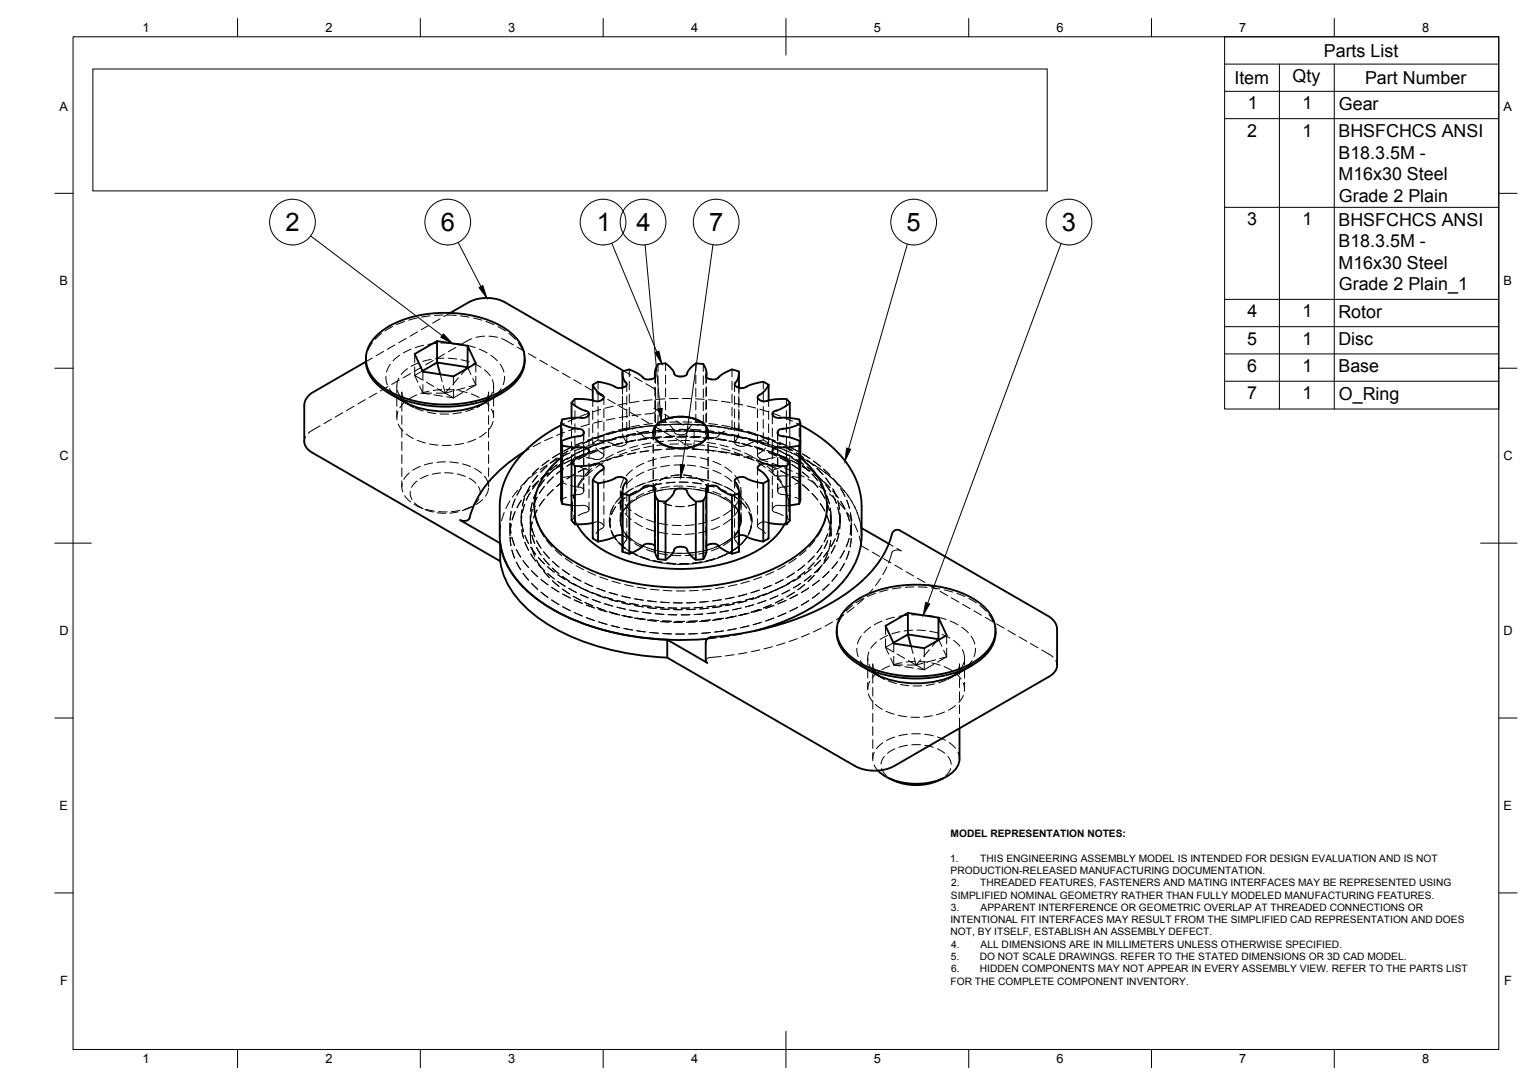
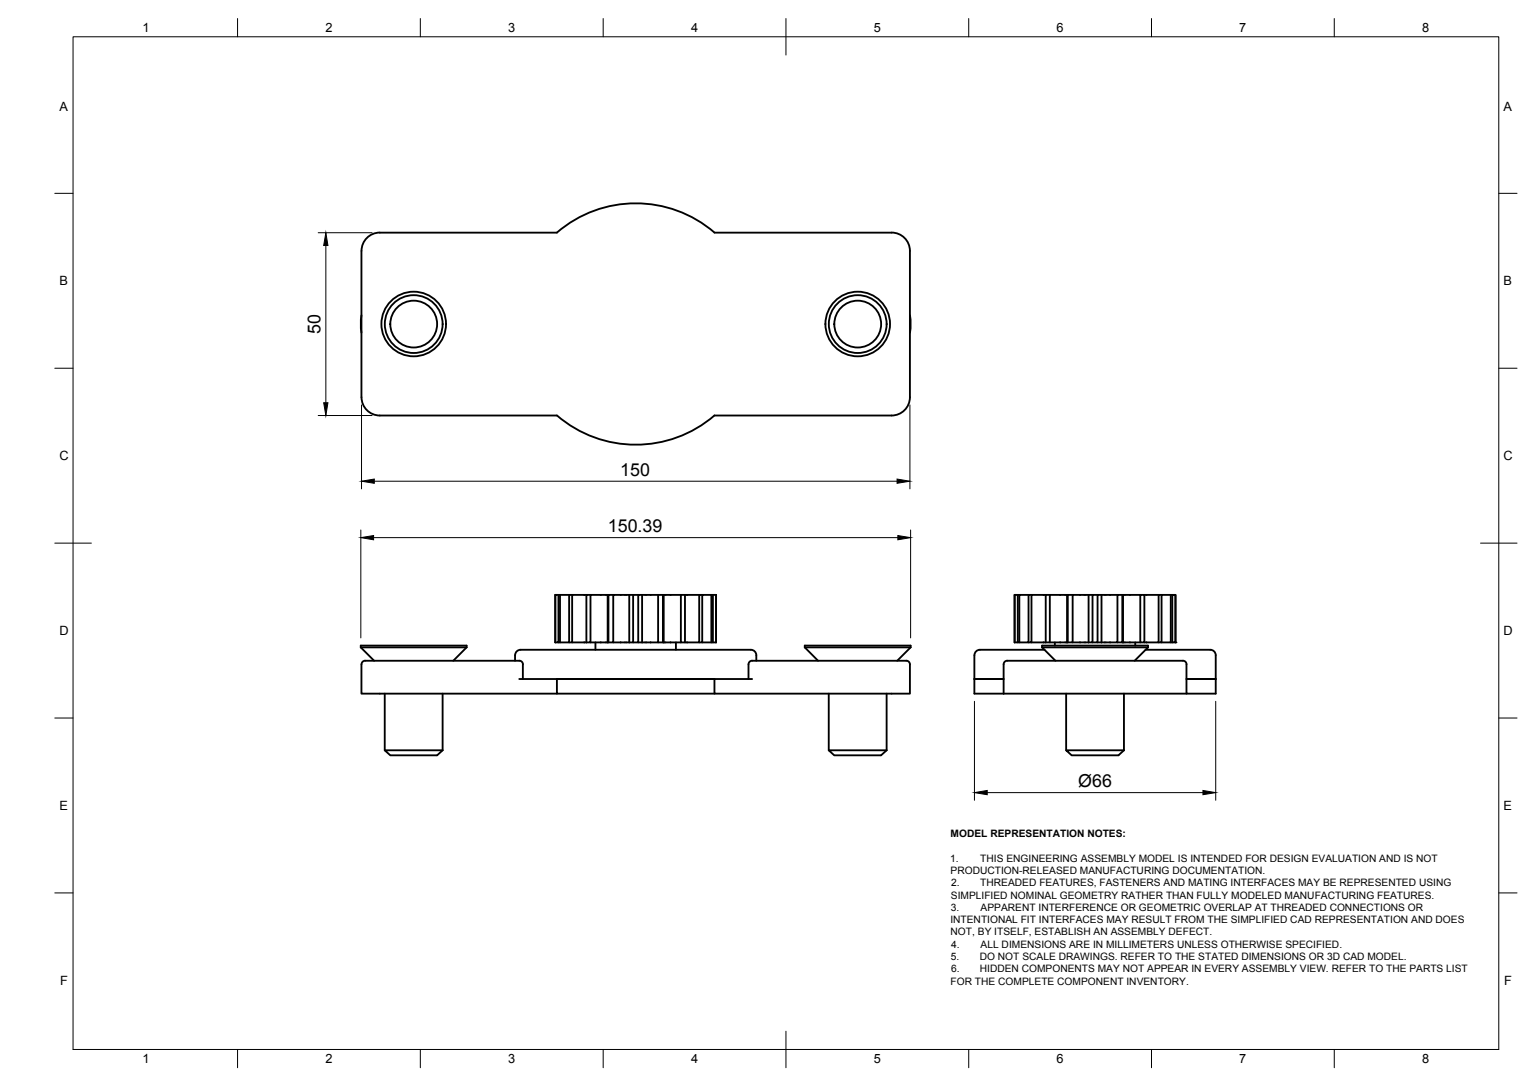
ISO-10303-21;
HEADER;
/* Generated by software containing ST-Developer
 * from STEP Tools, Inc. (www.steptools.com) 
 */

FILE_DESCRIPTION(
/* description */ (''),
/* implementation_level */ '2;1');

FILE_NAME(
/* name */ 'BR-110',
/* time_stamp */ '2026-10-04T22:47:03-07:00',
/* author */ (''),
/* organization */ (''),
/* preprocessor_version */ 'ST-DEVELOPER v20.2',
/* originating_system */ 'Autodesk Translation Framework v15.15.0.0',
/* authorisation */ '');

FILE_SCHEMA (('AUTOMOTIVE_DESIGN { 1 0 10303 214 3 1 1 }'));
ENDSEC;

DATA;
#10=MECHANICAL_DESIGN_GEOMETRIC_PRESENTATION_REPRESENTATION('',(#77,#78,
#79,#80,#81,#82,#83),#19878);
#11=ITEM_DEFINED_TRANSFORMATION($,$,#4911,#5420);
#12=ITEM_DEFINED_TRANSFORMATION($,$,#5197,#5421);
#13=ITEM_DEFINED_TRANSFORMATION($,$,#5224,#5422);
#14=ITEM_DEFINED_TRANSFORMATION($,$,#5251,#5423);
#15=ITEM_DEFINED_TRANSFORMATION($,$,#5268,#5424);
#16=ITEM_DEFINED_TRANSFORMATION($,$,#5309,#5425);
#17=ITEM_DEFINED_TRANSFORMATION($,$,#5416,#5426);
#18=(
REPRESENTATION_RELATIONSHIP($,$,#19907,#19906)
REPRESENTATION_RELATIONSHIP_WITH_TRANSFORMATION(#11)
SHAPE_REPRESENTATION_RELATIONSHIP()
);
#19=(
REPRESENTATION_RELATIONSHIP($,$,#19908,#19906)
REPRESENTATION_RELATIONSHIP_WITH_TRANSFORMATION(#12)
SHAPE_REPRESENTATION_RELATIONSHIP()
);
#20=(
REPRESENTATION_RELATIONSHIP($,$,#19909,#19906)
REPRESENTATION_RELATIONSHIP_WITH_TRANSFORMATION(#13)
SHAPE_REPRESENTATION_RELATIONSHIP()
);
#21=(
REPRESENTATION_RELATIONSHIP($,$,#19910,#19906)
REPRESENTATION_RELATIONSHIP_WITH_TRANSFORMATION(#14)
SHAPE_REPRESENTATION_RELATIONSHIP()
);
#22=(
REPRESENTATION_RELATIONSHIP($,$,#19911,#19906)
REPRESENTATION_RELATIONSHIP_WITH_TRANSFORMATION(#15)
SHAPE_REPRESENTATION_RELATIONSHIP()
);
#23=(
REPRESENTATION_RELATIONSHIP($,$,#19912,#19906)
REPRESENTATION_RELATIONSHIP_WITH_TRANSFORMATION(#16)
SHAPE_REPRESENTATION_RELATIONSHIP()
);
#24=(
REPRESENTATION_RELATIONSHIP($,$,#19913,#19906)
REPRESENTATION_RELATIONSHIP_WITH_TRANSFORMATION(#17)
SHAPE_REPRESENTATION_RELATIONSHIP()
);
#25=CONTEXT_DEPENDENT_SHAPE_REPRESENTATION(#18,#19899);
#26=CONTEXT_DEPENDENT_SHAPE_REPRESENTATION(#19,#19900);
#27=CONTEXT_DEPENDENT_SHAPE_REPRESENTATION(#20,#19901);
#28=CONTEXT_DEPENDENT_SHAPE_REPRESENTATION(#21,#19902);
#29=CONTEXT_DEPENDENT_SHAPE_REPRESENTATION(#22,#19903);
#30=CONTEXT_DEPENDENT_SHAPE_REPRESENTATION(#23,#19904);
#31=CONTEXT_DEPENDENT_SHAPE_REPRESENTATION(#24,#19905);
#32=NEXT_ASSEMBLY_USAGE_OCCURRENCE('Gear:1','Gear:1','Gear:1',#19915,#19916,
'Gear:1');
#33=NEXT_ASSEMBLY_USAGE_OCCURRENCE('Screw_02:1','Screw_02:1',
'Screw_02:1',#19915,#19917,'Screw_02:1');
#34=NEXT_ASSEMBLY_USAGE_OCCURRENCE('Screw_01:1','Screw_01:1',
'Screw_01:1',#19915,#19918,'Screw_01:1');
#35=NEXT_ASSEMBLY_USAGE_OCCURRENCE('Rotor:1','Rotor:1','Rotor:1',#19915,
#19919,'Rotor:1');
#36=NEXT_ASSEMBLY_USAGE_OCCURRENCE('Disc:1','Disc:1','Disc:1',#19915,#19920,
'Disc:1');
#37=NEXT_ASSEMBLY_USAGE_OCCURRENCE('Base:1','Base:1','Base:1',#19915,#19921,
'Base:1');
#38=NEXT_ASSEMBLY_USAGE_OCCURRENCE('O_Ring:1','O_Ring:1','O_Ring:1',#19915,
#19922,'O_Ring:1');
#39=SPHERICAL_SURFACE('',#5318,1.);
#40=SPHERICAL_SURFACE('',#5323,1.);
#41=SPHERICAL_SURFACE('',#5367,1.);
#42=SPHERICAL_SURFACE('',#5372,1.);
#43=TOROIDAL_SURFACE('',#5201,8.911,1.);
#44=TOROIDAL_SURFACE('',#5228,8.911,1.);
#45=TOROIDAL_SURFACE('',#5257,12.,1.);
#46=TOROIDAL_SURFACE('',#5269,18.2498324643894,1.5);
#47=TOROIDAL_SURFACE('',#5277,28.1934256722844,1.5);
#48=TOROIDAL_SURFACE('',#5285,31.5,1.5);
#49=TOROIDAL_SURFACE('',#5293,12.,1.);
#50=TOROIDAL_SURFACE('',#5313,39.889325151227,1.);
#51=TOROIDAL_SURFACE('',#5335,4.,1.);
#52=TOROIDAL_SURFACE('',#5340,4.,1.);
#53=TOROIDAL_SURFACE('',#5362,39.889325151227,1.);
#54=TOROIDAL_SURFACE('',#5384,4.,1.);
#55=TOROIDAL_SURFACE('',#5389,4.,1.);
#56=TOROIDAL_SURFACE('',#5417,12.,1.);
#57=CONICAL_SURFACE('',#5198,7.28,0.832981266674429);
#58=CONICAL_SURFACE('',#5205,11.24,0.785398163397495);
#59=CONICAL_SURFACE('',#5225,7.28,0.832981266674429);
#60=CONICAL_SURFACE('',#5232,11.24,0.785398163397495);
#61=CONICAL_SURFACE('',#5342,9.8273485245745,0.785398163397449);
#62=CONICAL_SURFACE('',#5391,9.8273485245745,0.785398163397449);
#63=SHAPE_REPRESENTATION_RELATIONSHIP('SRR','None',#19907,#70);
#64=SHAPE_REPRESENTATION_RELATIONSHIP('SRR','None',#19908,#71);
#65=SHAPE_REPRESENTATION_RELATIONSHIP('SRR','None',#19909,#72);
#66=SHAPE_REPRESENTATION_RELATIONSHIP('SRR','None',#19910,#73);
#67=SHAPE_REPRESENTATION_RELATIONSHIP('SRR','None',#19911,#74);
#68=SHAPE_REPRESENTATION_RELATIONSHIP('SRR','None',#19912,#75);
#69=SHAPE_REPRESENTATION_RELATIONSHIP('SRR','None',#19913,#76);
#70=ADVANCED_BREP_SHAPE_REPRESENTATION('',(#84),#19871);
#71=ADVANCED_BREP_SHAPE_REPRESENTATION('',(#85),#19872);
#72=ADVANCED_BREP_SHAPE_REPRESENTATION('',(#86),#19873);
#73=ADVANCED_BREP_SHAPE_REPRESENTATION('',(#87),#19874);
#74=ADVANCED_BREP_SHAPE_REPRESENTATION('',(#88),#19875);
#75=ADVANCED_BREP_SHAPE_REPRESENTATION('',(#89),#19876);
#76=ADVANCED_BREP_SHAPE_REPRESENTATION('',(#90),#19877);
#77=STYLED_ITEM('',(#19951),#84);
#78=STYLED_ITEM('',(#19952),#85);
#79=STYLED_ITEM('',(#19952),#86);
#80=STYLED_ITEM('',(#19953),#87);
#81=STYLED_ITEM('',(#19954),#88);
#82=STYLED_ITEM('',(#19951),#89);
#83=STYLED_ITEM('',(#19955),#90);
#84=MANIFOLD_SOLID_BREP('Body1',#4825);
#85=MANIFOLD_SOLID_BREP('Body1',#4826);
#86=MANIFOLD_SOLID_BREP('Body1',#4827);
#87=MANIFOLD_SOLID_BREP('Body1',#4828);
#88=MANIFOLD_SOLID_BREP('Body1',#4829);
#89=MANIFOLD_SOLID_BREP('Body1',#4830);
#90=MANIFOLD_SOLID_BREP('Body1',#4831);
#91=FACE_BOUND('',#736,.T.);
#92=FACE_BOUND('',#738,.T.);
#93=FACE_BOUND('',#783,.T.);
#94=FACE_BOUND('',#803,.T.);
#95=FACE_BOUND('',#808,.T.);
#96=FACE_BOUND('',#814,.T.);
#97=FACE_BOUND('',#819,.T.);
#98=FACE_BOUND('',#822,.T.);
#99=FACE_BOUND('',#827,.T.);
#100=FACE_BOUND('',#831,.T.);
#101=FACE_BOUND('',#834,.T.);
#102=FACE_BOUND('',#837,.T.);
#103=FACE_BOUND('',#840,.T.);
#104=FACE_BOUND('',#849,.T.);
#105=FACE_BOUND('',#871,.T.);
#106=FACE_BOUND('',#886,.T.);
#107=FACE_BOUND('',#887,.T.);
#108=FACE_BOUND('',#889,.T.);
#109=FACE_BOUND('',#892,.T.);
#110=FACE_BOUND('',#895,.T.);
#111=B_SPLINE_CURVE_WITH_KNOTS('',5,(#7546,#7547,#7548,#7549,#7550,#7551,
#7552,#7553,#7554,#7555,#7556,#7557,#7558,#7559,#7560,#7561,#7562,#7563,
#7564,#7565,#7566,#7567,#7568,#7569,#7570,#7571,#7572,#7573,#7574,#7575,
#7576,#7577,#7578,#7579,#7580,#7581,#7582,#7583,#7584,#7585,#7586,#7587,
#7588,#7589,#7590,#7591,#7592,#7593,#7594,#7595,#7596,#7597,#7598,#7599,
#7600,#7601,#7602,#7603,#7604,#7605,#7606,#7607,#7608,#7609,#7610,#7611,
#7612,#7613,#7614,#7615,#7616,#7617,#7618,#7619),.UNSPECIFIED.,.F.,.F.,
(6,1,1,1,1,1,1,1,1,1,1,1,1,1,1,1,1,1,1,1,1,1,1,1,1,1,1,1,1,1,1,1,1,1,1,
1,1,1,1,1,1,1,1,1,1,1,1,1,1,1,1,1,1,1,1,1,1,1,1,1,1,1,1,1,1,1,1,1,1,6),
(0.,0.0142857142857143,0.0285714285714286,0.0428571428571429,0.0571428571428571,
0.0714285714285714,0.0857142857142857,0.1,0.114285714285714,0.128571428571429,
0.142857142857143,0.157142857142857,0.171428571428571,0.185714285714286,
0.2,0.214285714285714,0.228571428571429,0.242857142857143,0.257142857142857,
0.271428571428571,0.285714285714286,0.3,0.314285714285714,0.328571428571429,
0.342857142857143,0.357142857142857,0.371428571428571,0.385714285714286,
0.4,0.414285714285714,0.428571428571429,0.442857142857143,0.457142857142857,
0.471428571428572,0.485714285714286,0.5,0.514285714285714,0.528571428571429,
0.542857142857143,0.557142857142857,0.571428571428571,0.585714285714286,
0.6,0.614285714285714,0.628571428571428,0.642857142857142,0.657142857142857,
0.671428571428571,0.685714285714285,0.699999999999999,0.714285714285714,
0.728571428571428,0.742857142857142,0.757142857142856,0.771428571428571,
0.785714285714285,0.799999999999999,0.814285714285713,0.828571428571428,
0.842857142857142,0.857142857142856,0.87142857142857,0.885714285714284,
0.899999999999999,0.914285714285713,0.928571428571427,0.942857142857141,
0.957142857142856,0.97142857142857,1.),.UNSPECIFIED.);
#112=B_SPLINE_CURVE_WITH_KNOTS('',3,(#7621,#7622,#7623,#7624,#7625,#7626,
#7627,#7628,#7629,#7630,#7631,#7632,#7633,#7634,#7635,#7636,#7637,#7638,
#7639,#7640,#7641,#7642,#7643,#7644,#7645,#7646,#7647,#7648,#7649,#7650,
#7651,#7652,#7653,#7654,#7655,#7656,#7657,#7658,#7659,#7660,#7661,#7662,
#7663,#7664,#7665,#7666,#7667,#7668,#7669,#7670,#7671,#7672,#7673,#7674,
#7675,#7676,#7677,#7678,#7679,#7680,#7681,#7682,#7683,#7684,#7685,#7686,
#7687),.UNSPECIFIED.,.F.,.F.,(4,3,3,3,3,3,3,3,3,3,3,3,3,3,3,3,3,3,3,3,3,
3,4),(-0.0308474254321917,-0.0282443140955979,-0.0239308458396743,-0.020615261220034,
-0.0170461143578005,-0.0150701375986627,-0.0131660090560162,-0.0115202579240142,
-0.0103391768048034,-0.00917732809651329,-0.00816993701567056,-0.00725747184422916,
-0.00648885937671962,-0.00537659348714137,-0.0047045193012487,-0.00408467783345363,
-0.00323202309358667,-0.00269108370723003,-0.00220561578671065,-0.00169529231611998,
-0.000847646158059989,-0.000380223899959456,0.),.UNSPECIFIED.);
#113=B_SPLINE_CURVE_WITH_KNOTS('',5,(#7845,#7846,#7847,#7848,#7849,#7850,
#7851,#7852,#7853,#7854,#7855,#7856,#7857,#7858,#7859,#7860,#7861,#7862,
#7863,#7864,#7865,#7866,#7867,#7868,#7869,#7870,#7871,#7872,#7873,#7874,
#7875,#7876,#7877,#7878,#7879,#7880,#7881,#7882,#7883,#7884,#7885,#7886,
#7887,#7888,#7889,#7890,#7891,#7892,#7893,#7894,#7895,#7896,#7897,#7898,
#7899,#7900,#7901,#7902,#7903,#7904,#7905,#7906,#7907,#7908,#7909,#7910,
#7911,#7912,#7913,#7914,#7915,#7916,#7917,#7918),.UNSPECIFIED.,.F.,.F.,
(6,1,1,1,1,1,1,1,1,1,1,1,1,1,1,1,1,1,1,1,1,1,1,1,1,1,1,1,1,1,1,1,1,1,1,
1,1,1,1,1,1,1,1,1,1,1,1,1,1,1,1,1,1,1,1,1,1,1,1,1,1,1,1,1,1,1,1,1,1,6),
(0.,0.0142857142857143,0.0285714285714286,0.0428571428571429,0.0571428571428571,
0.0714285714285714,0.0857142857142857,0.1,0.114285714285714,0.128571428571429,
0.142857142857143,0.157142857142857,0.171428571428571,0.185714285714286,
0.2,0.214285714285714,0.228571428571429,0.242857142857143,0.257142857142857,
0.271428571428571,0.285714285714286,0.3,0.314285714285714,0.328571428571429,
0.342857142857143,0.357142857142857,0.371428571428571,0.385714285714286,
0.4,0.414285714285714,0.428571428571429,0.442857142857143,0.457142857142857,
0.471428571428572,0.485714285714286,0.5,0.514285714285714,0.528571428571429,
0.542857142857143,0.557142857142857,0.571428571428571,0.585714285714286,
0.6,0.614285714285714,0.628571428571428,0.642857142857142,0.657142857142857,
0.671428571428571,0.685714285714285,0.699999999999999,0.714285714285714,
0.728571428571428,0.742857142857142,0.757142857142856,0.771428571428571,
0.785714285714285,0.799999999999999,0.814285714285713,0.828571428571428,
0.842857142857142,0.857142857142856,0.87142857142857,0.885714285714284,
0.899999999999999,0.914285714285713,0.928571428571427,0.942857142857141,
0.957142857142856,0.97142857142857,1.),.UNSPECIFIED.);
#114=B_SPLINE_CURVE_WITH_KNOTS('',3,(#7919,#7920,#7921,#7922,#7923,#7924,
#7925,#7926,#7927,#7928,#7929,#7930,#7931,#7932,#7933,#7934,#7935,#7936,
#7937,#7938,#7939,#7940,#7941,#7942,#7943,#7944,#7945,#7946,#7947,#7948,
#7949,#7950,#7951,#7952,#7953,#7954,#7955,#7956,#7957,#7958,#7959,#7960,
#7961,#7962,#7963,#7964,#7965,#7966,#7967,#7968,#7969,#7970,#7971,#7972,
#7973,#7974,#7975,#7976,#7977,#7978,#7979,#7980,#7981,#7982,#7983,#7984,
#7985,#7986,#7987,#7988),.UNSPECIFIED.,.F.,.F.,(4,3,3,3,3,3,3,3,3,3,3,3,
3,3,3,3,3,3,3,3,3,3,3,4),(-0.41144900970185,-0.405504895343942,-0.398537948713814,
-0.388735121356617,-0.382214695160452,-0.375350877738258,-0.367728232762158,
-0.356236725488341,-0.34788839668605,-0.33768327957583,-0.326660059396151,
-0.316483474305328,-0.302658060948649,-0.289316835657715,-0.271192407308052,
-0.255261428784221,-0.231775298718215,-0.202135573387617,-0.16198628027827,
-0.126192134079699,-0.0754619858625935,-0.0360560120089752,-0.00196686783518586,
0.),.UNSPECIFIED.);
#115=B_SPLINE_CURVE_WITH_KNOTS('',5,(#8140,#8141,#8142,#8143,#8144,#8145,
#8146,#8147,#8148,#8149,#8150,#8151,#8152,#8153,#8154,#8155,#8156,#8157,
#8158,#8159,#8160,#8161,#8162,#8163,#8164,#8165,#8166,#8167,#8168,#8169,
#8170,#8171,#8172,#8173,#8174,#8175,#8176,#8177,#8178,#8179,#8180,#8181,
#8182,#8183,#8184,#8185,#8186,#8187,#8188,#8189,#8190,#8191,#8192,#8193,
#8194,#8195,#8196,#8197,#8198,#8199,#8200,#8201,#8202,#8203,#8204,#8205,
#8206,#8207,#8208,#8209,#8210,#8211,#8212,#8213),.UNSPECIFIED.,.F.,.F.,
(6,1,1,1,1,1,1,1,1,1,1,1,1,1,1,1,1,1,1,1,1,1,1,1,1,1,1,1,1,1,1,1,1,1,1,
1,1,1,1,1,1,1,1,1,1,1,1,1,1,1,1,1,1,1,1,1,1,1,1,1,1,1,1,1,1,1,1,1,1,6),
(0.,0.0142857142857143,0.0285714285714286,0.0428571428571429,0.0571428571428571,
0.0714285714285714,0.0857142857142857,0.1,0.114285714285714,0.128571428571429,
0.142857142857143,0.157142857142857,0.171428571428571,0.185714285714286,
0.2,0.214285714285714,0.228571428571429,0.242857142857143,0.257142857142857,
0.271428571428571,0.285714285714286,0.3,0.314285714285714,0.328571428571429,
0.342857142857143,0.357142857142857,0.371428571428571,0.385714285714286,
0.4,0.414285714285714,0.428571428571429,0.442857142857143,0.457142857142857,
0.471428571428572,0.485714285714286,0.5,0.514285714285714,0.528571428571429,
0.542857142857143,0.557142857142857,0.571428571428571,0.585714285714286,
0.6,0.614285714285714,0.628571428571428,0.642857142857142,0.657142857142857,
0.671428571428571,0.685714285714285,0.699999999999999,0.714285714285714,
0.728571428571428,0.742857142857142,0.757142857142856,0.771428571428571,
0.785714285714285,0.799999999999999,0.814285714285713,0.828571428571428,
0.842857142857142,0.857142857142856,0.87142857142857,0.885714285714284,
0.899999999999999,0.914285714285713,0.928571428571427,0.942857142857141,
0.957142857142856,0.97142857142857,1.),.UNSPECIFIED.);
#116=B_SPLINE_CURVE_WITH_KNOTS('',3,(#8215,#8216,#8217,#8218,#8219,#8220,
#8221,#8222,#8223,#8224,#8225,#8226,#8227,#8228,#8229,#8230,#8231,#8232,
#8233,#8234,#8235,#8236,#8237,#8238,#8239,#8240,#8241,#8242,#8243,#8244,
#8245,#8246,#8247,#8248,#8249,#8250,#8251,#8252,#8253,#8254,#8255,#8256,
#8257,#8258,#8259,#8260,#8261,#8262,#8263,#8264,#8265,#8266,#8267,#8268,
#8269,#8270,#8271,#8272,#8273,#8274,#8275,#8276,#8277,#8278,#8279,#8280,
#8281),.UNSPECIFIED.,.F.,.F.,(4,3,3,3,3,3,3,3,3,3,3,3,3,3,3,3,3,3,3,3,3,
3,4),(-0.0308474253927552,-0.0282443143977923,-0.0239308462347147,-0.0206152615976367,
-0.017046114438784,-0.0150701378006816,-0.0131660089382207,-0.0115202578209431,
-0.0103391766998121,-0.00917732804029983,-0.00816993698852514,-0.00725747180050917,
-0.00648885933763945,-0.00537659350788907,-0.00470451931940294,-0.00408467785449232,
-0.00323202307997564,-0.00269108369563703,-0.00220561577615339,-0.00169529230461842,
-0.000847646152309211,-0.000380223895211713,0.),.UNSPECIFIED.);
#117=B_SPLINE_CURVE_WITH_KNOTS('',5,(#8439,#8440,#8441,#8442,#8443,#8444,
#8445,#8446,#8447,#8448,#8449,#8450,#8451,#8452,#8453,#8454,#8455,#8456,
#8457,#8458,#8459,#8460,#8461,#8462,#8463,#8464,#8465,#8466,#8467,#8468,
#8469,#8470,#8471,#8472,#8473,#8474,#8475,#8476,#8477,#8478,#8479,#8480,
#8481,#8482,#8483,#8484,#8485,#8486,#8487,#8488,#8489,#8490,#8491,#8492,
#8493,#8494,#8495,#8496,#8497,#8498,#8499,#8500,#8501,#8502,#8503,#8504,
#8505,#8506,#8507,#8508,#8509,#8510,#8511,#8512),.UNSPECIFIED.,.F.,.F.,
(6,1,1,1,1,1,1,1,1,1,1,1,1,1,1,1,1,1,1,1,1,1,1,1,1,1,1,1,1,1,1,1,1,1,1,
1,1,1,1,1,1,1,1,1,1,1,1,1,1,1,1,1,1,1,1,1,1,1,1,1,1,1,1,1,1,1,1,1,1,6),
(0.,0.0142857142857143,0.0285714285714286,0.0428571428571429,0.0571428571428571,
0.0714285714285714,0.0857142857142857,0.1,0.114285714285714,0.128571428571429,
0.142857142857143,0.157142857142857,0.171428571428571,0.185714285714286,
0.2,0.214285714285714,0.228571428571429,0.242857142857143,0.257142857142857,
0.271428571428571,0.285714285714286,0.3,0.314285714285714,0.328571428571429,
0.342857142857143,0.357142857142857,0.371428571428571,0.385714285714286,
0.4,0.414285714285714,0.428571428571429,0.442857142857143,0.457142857142857,
0.471428571428572,0.485714285714286,0.5,0.514285714285714,0.528571428571429,
0.542857142857143,0.557142857142857,0.571428571428571,0.585714285714286,
0.6,0.614285714285714,0.628571428571428,0.642857142857142,0.657142857142857,
0.671428571428571,0.685714285714285,0.699999999999999,0.714285714285714,
0.728571428571428,0.742857142857142,0.757142857142856,0.771428571428571,
0.785714285714285,0.799999999999999,0.814285714285713,0.828571428571428,
0.842857142857142,0.857142857142856,0.87142857142857,0.885714285714284,
0.899999999999999,0.914285714285713,0.928571428571427,0.942857142857141,
0.957142857142856,0.97142857142857,1.),.UNSPECIFIED.);
#118=B_SPLINE_CURVE_WITH_KNOTS('',3,(#8513,#8514,#8515,#8516,#8517,#8518,
#8519,#8520,#8521,#8522,#8523,#8524,#8525,#8526,#8527,#8528,#8529,#8530,
#8531,#8532,#8533,#8534,#8535,#8536,#8537,#8538,#8539,#8540,#8541,#8542,
#8543,#8544,#8545,#8546,#8547,#8548,#8549,#8550,#8551,#8552,#8553,#8554,
#8555,#8556,#8557,#8558,#8559,#8560,#8561,#8562,#8563,#8564,#8565,#8566,
#8567,#8568,#8569,#8570,#8571,#8572,#8573,#8574,#8575,#8576,#8577,#8578,
#8579,#8580,#8581,#8582,#8583,#8584,#8585,#8586,#8587,#8588),
 .UNSPECIFIED.,.F.,.F.,(4,3,3,3,3,3,3,3,3,3,3,3,3,3,3,3,3,3,3,3,3,3,3,3,
3,4),(-0.411449009835962,-0.403601796399829,-0.395573025581345,-0.386876504715203,
-0.375226575568619,-0.367043560841026,-0.358155681265519,-0.345047445919287,
-0.335636642409539,-0.325415895835815,-0.30690198526545,-0.293588015170367,
-0.286320302426775,-0.284969138437181,-0.283753083910261,-0.264146344834336,
-0.2466687814383,-0.228881898831898,-0.20935255979658,-0.188662818643314,
-0.1773046112729,-0.142988917240362,-0.110440538152722,-0.0644976592576526,
-0.0288887144369996,0.),.UNSPECIFIED.);
#119=B_SPLINE_CURVE_WITH_KNOTS('',5,(#8740,#8741,#8742,#8743,#8744,#8745,
#8746,#8747,#8748,#8749,#8750,#8751,#8752,#8753,#8754,#8755,#8756,#8757,
#8758,#8759,#8760,#8761,#8762,#8763,#8764,#8765,#8766,#8767,#8768,#8769,
#8770,#8771,#8772,#8773,#8774,#8775,#8776,#8777,#8778,#8779,#8780,#8781,
#8782,#8783,#8784,#8785,#8786,#8787,#8788,#8789,#8790,#8791,#8792,#8793,
#8794,#8795,#8796,#8797,#8798,#8799,#8800,#8801,#8802,#8803,#8804,#8805,
#8806,#8807,#8808,#8809,#8810,#8811,#8812,#8813),.UNSPECIFIED.,.F.,.F.,
(6,1,1,1,1,1,1,1,1,1,1,1,1,1,1,1,1,1,1,1,1,1,1,1,1,1,1,1,1,1,1,1,1,1,1,
1,1,1,1,1,1,1,1,1,1,1,1,1,1,1,1,1,1,1,1,1,1,1,1,1,1,1,1,1,1,1,1,1,1,6),
(0.,0.0142857142857143,0.0285714285714286,0.0428571428571429,0.0571428571428571,
0.0714285714285714,0.0857142857142857,0.1,0.114285714285714,0.128571428571429,
0.142857142857143,0.157142857142857,0.171428571428571,0.185714285714286,
0.2,0.214285714285714,0.228571428571429,0.242857142857143,0.257142857142857,
0.271428571428571,0.285714285714286,0.3,0.314285714285714,0.328571428571429,
0.342857142857143,0.357142857142857,0.371428571428571,0.385714285714286,
0.4,0.414285714285714,0.428571428571429,0.442857142857143,0.457142857142857,
0.471428571428572,0.485714285714286,0.5,0.514285714285714,0.528571428571429,
0.542857142857143,0.557142857142857,0.571428571428571,0.585714285714286,
0.6,0.614285714285714,0.628571428571428,0.642857142857142,0.657142857142857,
0.671428571428571,0.685714285714285,0.699999999999999,0.714285714285714,
0.728571428571428,0.742857142857142,0.757142857142856,0.771428571428571,
0.785714285714285,0.799999999999999,0.814285714285713,0.828571428571428,
0.842857142857142,0.857142857142856,0.87142857142857,0.885714285714284,
0.899999999999999,0.914285714285713,0.928571428571427,0.942857142857141,
0.957142857142856,0.97142857142857,1.),.UNSPECIFIED.);
#120=B_SPLINE_CURVE_WITH_KNOTS('',3,(#8815,#8816,#8817,#8818,#8819,#8820,
#8821,#8822,#8823,#8824,#8825,#8826,#8827,#8828,#8829,#8830,#8831,#8832,
#8833,#8834,#8835,#8836,#8837,#8838,#8839,#8840,#8841,#8842,#8843,#8844,
#8845,#8846,#8847,#8848,#8849,#8850,#8851,#8852,#8853,#8854,#8855,#8856,
#8857,#8858,#8859,#8860,#8861,#8862,#8863,#8864,#8865,#8866,#8867,#8868,
#8869,#8870,#8871,#8872,#8873,#8874,#8875,#8876,#8877,#8878,#8879,#8880,
#8881),.UNSPECIFIED.,.F.,.F.,(4,3,3,3,3,3,3,3,3,3,3,3,3,3,3,3,3,3,3,3,3,
3,4),(-0.0308474254458724,-0.0282443139325418,-0.0239308456237518,-0.0206152609798776,
-0.0170461143209945,-0.0150701375196663,-0.0131660090920878,-0.0115202579555768,
-0.0103391768402169,-0.00917732811491881,-0.00816993702510001,-0.00725747186261159,
-0.0064888593923997,-0.00537659347817632,-0.00470451929340428,-0.00408467782457058,
-0.0032320230991173,-0.00269108371201768,-0.00220561579110508,-0.00169529232104257,
-0.000847646160521286,-0.000380223902305551,0.),.UNSPECIFIED.);
#121=B_SPLINE_CURVE_WITH_KNOTS('',5,(#9039,#9040,#9041,#9042,#9043,#9044,
#9045,#9046,#9047,#9048,#9049,#9050,#9051,#9052,#9053,#9054,#9055,#9056,
#9057,#9058,#9059,#9060,#9061,#9062,#9063,#9064,#9065,#9066,#9067,#9068,
#9069,#9070,#9071,#9072,#9073,#9074,#9075,#9076,#9077,#9078,#9079,#9080,
#9081,#9082,#9083,#9084,#9085,#9086,#9087,#9088,#9089,#9090,#9091,#9092,
#9093,#9094,#9095,#9096,#9097,#9098,#9099,#9100,#9101,#9102,#9103,#9104,
#9105,#9106,#9107,#9108,#9109,#9110,#9111,#9112),.UNSPECIFIED.,.F.,.F.,
(6,1,1,1,1,1,1,1,1,1,1,1,1,1,1,1,1,1,1,1,1,1,1,1,1,1,1,1,1,1,1,1,1,1,1,
1,1,1,1,1,1,1,1,1,1,1,1,1,1,1,1,1,1,1,1,1,1,1,1,1,1,1,1,1,1,1,1,1,1,6),
(0.,0.0142857142857143,0.0285714285714286,0.0428571428571429,0.0571428571428571,
0.0714285714285714,0.0857142857142857,0.1,0.114285714285714,0.128571428571429,
0.142857142857143,0.157142857142857,0.171428571428571,0.185714285714286,
0.2,0.214285714285714,0.228571428571429,0.242857142857143,0.257142857142857,
0.271428571428571,0.285714285714286,0.3,0.314285714285714,0.328571428571429,
0.342857142857143,0.357142857142857,0.371428571428571,0.385714285714286,
0.4,0.414285714285714,0.428571428571429,0.442857142857143,0.457142857142857,
0.471428571428572,0.485714285714286,0.5,0.514285714285714,0.528571428571429,
0.542857142857143,0.557142857142857,0.571428571428571,0.585714285714286,
0.6,0.614285714285714,0.628571428571428,0.642857142857142,0.657142857142857,
0.671428571428571,0.685714285714285,0.699999999999999,0.714285714285714,
0.728571428571428,0.742857142857142,0.757142857142856,0.771428571428571,
0.785714285714285,0.799999999999999,0.814285714285713,0.828571428571428,
0.842857142857142,0.857142857142856,0.87142857142857,0.885714285714284,
0.899999999999999,0.914285714285713,0.928571428571427,0.942857142857141,
0.957142857142856,0.97142857142857,1.),.UNSPECIFIED.);
#122=B_SPLINE_CURVE_WITH_KNOTS('',3,(#9113,#9114,#9115,#9116,#9117,#9118,
#9119,#9120,#9121,#9122,#9123,#9124,#9125,#9126,#9127,#9128,#9129,#9130,
#9131,#9132,#9133,#9134,#9135,#9136,#9137,#9138,#9139,#9140,#9141,#9142,
#9143,#9144,#9145,#9146,#9147,#9148,#9149,#9150,#9151,#9152,#9153,#9154,
#9155,#9156,#9157,#9158,#9159,#9160,#9161,#9162,#9163,#9164,#9165,#9166,
#9167,#9168,#9169,#9170,#9171,#9172,#9173,#9174,#9175,#9176,#9177,#9178,
#9179,#9180,#9181,#9182),.UNSPECIFIED.,.F.,.F.,(4,3,3,3,3,3,3,3,3,3,3,3,
3,3,3,3,3,3,3,3,3,3,3,4),(-0.411449010058416,-0.405504895678982,-0.398537949040723,
-0.388735121700349,-0.382214695498563,-0.375350878070222,-0.367728233088589,
-0.356236725804571,-0.347888396993553,-0.337683279874044,-0.326660059681915,
-0.316483474587148,-0.302658061236691,-0.289316835946338,-0.271192407689148,
-0.25526142925369,-0.231775299041798,-0.202135573687089,-0.161986280481546,
-0.126192134078593,-0.075461985765785,-0.0360560137735561,-0.00196687385551187,
0.),.UNSPECIFIED.);
#123=B_SPLINE_CURVE_WITH_KNOTS('',5,(#9334,#9335,#9336,#9337,#9338,#9339,
#9340,#9341,#9342,#9343,#9344,#9345,#9346,#9347,#9348,#9349,#9350,#9351,
#9352,#9353,#9354,#9355,#9356,#9357,#9358,#9359,#9360,#9361,#9362,#9363,
#9364,#9365,#9366,#9367,#9368,#9369,#9370,#9371,#9372,#9373,#9374,#9375,
#9376,#9377,#9378,#9379,#9380,#9381,#9382,#9383,#9384,#9385,#9386,#9387,
#9388,#9389,#9390,#9391,#9392,#9393,#9394,#9395,#9396,#9397,#9398,#9399,
#9400,#9401,#9402,#9403,#9404,#9405,#9406,#9407),.UNSPECIFIED.,.F.,.F.,
(6,1,1,1,1,1,1,1,1,1,1,1,1,1,1,1,1,1,1,1,1,1,1,1,1,1,1,1,1,1,1,1,1,1,1,
1,1,1,1,1,1,1,1,1,1,1,1,1,1,1,1,1,1,1,1,1,1,1,1,1,1,1,1,1,1,1,1,1,1,6),
(0.,0.0142857142857143,0.0285714285714286,0.0428571428571429,0.0571428571428571,
0.0714285714285714,0.0857142857142857,0.1,0.114285714285714,0.128571428571429,
0.142857142857143,0.157142857142857,0.171428571428571,0.185714285714286,
0.2,0.214285714285714,0.228571428571429,0.242857142857143,0.257142857142857,
0.271428571428571,0.285714285714286,0.3,0.314285714285714,0.328571428571429,
0.342857142857143,0.357142857142857,0.371428571428571,0.385714285714286,
0.4,0.414285714285714,0.428571428571429,0.442857142857143,0.457142857142857,
0.471428571428572,0.485714285714286,0.5,0.514285714285714,0.528571428571429,
0.542857142857143,0.557142857142857,0.571428571428571,0.585714285714286,
0.6,0.614285714285714,0.628571428571428,0.642857142857142,0.657142857142857,
0.671428571428571,0.685714285714285,0.699999999999999,0.714285714285714,
0.728571428571428,0.742857142857142,0.757142857142856,0.771428571428571,
0.785714285714285,0.799999999999999,0.814285714285713,0.828571428571428,
0.842857142857142,0.857142857142856,0.87142857142857,0.885714285714284,
0.899999999999999,0.914285714285713,0.928571428571427,0.942857142857141,
0.957142857142856,0.97142857142857,1.),.UNSPECIFIED.);
#124=B_SPLINE_CURVE_WITH_KNOTS('',3,(#9409,#9410,#9411,#9412,#9413,#9414,
#9415,#9416,#9417,#9418,#9419,#9420,#9421,#9422,#9423,#9424,#9425,#9426,
#9427,#9428,#9429,#9430,#9431,#9432,#9433,#9434,#9435,#9436,#9437,#9438,
#9439,#9440,#9441,#9442,#9443,#9444,#9445,#9446,#9447,#9448,#9449,#9450,
#9451,#9452,#9453,#9454,#9455,#9456,#9457,#9458,#9459,#9460,#9461,#9462,
#9463,#9464,#9465,#9466,#9467,#9468,#9469,#9470,#9471,#9472,#9473,#9474,
#9475),.UNSPECIFIED.,.F.,.F.,(4,3,3,3,3,3,3,3,3,3,3,3,3,3,3,3,3,3,3,3,3,
3,4),(-0.0308474254450083,-0.0282443143076938,-0.0239308461003898,-0.0206152614713912,
-0.0170461144298779,-0.0150701377273182,-0.0131660090093565,-0.0115202578831869,
-0.0103391767614099,-0.00917732807782989,-0.00816993701064961,-0.00725747183277268,
-0.00648885936633748,-0.00537659350089532,-0.00470451931328341,-0.00408467784616126,
-0.00323202309082144,-0.00269108370483176,-0.00220561578430491,-0.0016952923129278,
-0.000847646156463901,-0.000380223898998028,0.),.UNSPECIFIED.);
#125=B_SPLINE_CURVE_WITH_KNOTS('',5,(#9633,#9634,#9635,#9636,#9637,#9638,
#9639,#9640,#9641,#9642,#9643,#9644,#9645,#9646,#9647,#9648,#9649,#9650,
#9651,#9652,#9653,#9654,#9655,#9656,#9657,#9658,#9659,#9660,#9661,#9662,
#9663,#9664,#9665,#9666,#9667,#9668,#9669,#9670,#9671,#9672,#9673,#9674,
#9675,#9676,#9677,#9678,#9679,#9680,#9681,#9682,#9683,#9684,#9685,#9686,
#9687,#9688,#9689,#9690,#9691,#9692,#9693,#9694,#9695,#9696,#9697,#9698,
#9699,#9700,#9701,#9702,#9703,#9704,#9705,#9706),.UNSPECIFIED.,.F.,.F.,
(6,1,1,1,1,1,1,1,1,1,1,1,1,1,1,1,1,1,1,1,1,1,1,1,1,1,1,1,1,1,1,1,1,1,1,
1,1,1,1,1,1,1,1,1,1,1,1,1,1,1,1,1,1,1,1,1,1,1,1,1,1,1,1,1,1,1,1,1,1,6),
(0.,0.0142857142857143,0.0285714285714286,0.0428571428571429,0.0571428571428571,
0.0714285714285714,0.0857142857142857,0.1,0.114285714285714,0.128571428571429,
0.142857142857143,0.157142857142857,0.171428571428571,0.185714285714286,
0.2,0.214285714285714,0.228571428571429,0.242857142857143,0.257142857142857,
0.271428571428571,0.285714285714286,0.3,0.314285714285714,0.328571428571429,
0.342857142857143,0.357142857142857,0.371428571428571,0.385714285714286,
0.4,0.414285714285714,0.428571428571429,0.442857142857143,0.457142857142857,
0.471428571428572,0.485714285714286,0.5,0.514285714285714,0.528571428571429,
0.542857142857143,0.557142857142857,0.571428571428571,0.585714285714286,
0.6,0.614285714285714,0.628571428571428,0.642857142857142,0.657142857142857,
0.671428571428571,0.685714285714285,0.699999999999999,0.714285714285714,
0.728571428571428,0.742857142857142,0.757142857142856,0.771428571428571,
0.785714285714285,0.799999999999999,0.814285714285713,0.828571428571428,
0.842857142857142,0.857142857142856,0.87142857142857,0.885714285714284,
0.899999999999999,0.914285714285713,0.928571428571427,0.942857142857141,
0.957142857142856,0.97142857142857,1.),.UNSPECIFIED.);
#126=B_SPLINE_CURVE_WITH_KNOTS('',3,(#9707,#9708,#9709,#9710,#9711,#9712,
#9713,#9714,#9715,#9716,#9717,#9718,#9719,#9720,#9721,#9722,#9723,#9724,
#9725,#9726,#9727,#9728,#9729,#9730,#9731,#9732,#9733,#9734,#9735,#9736,
#9737,#9738,#9739,#9740,#9741,#9742,#9743,#9744,#9745,#9746,#9747,#9748,
#9749,#9750,#9751,#9752,#9753,#9754,#9755,#9756,#9757,#9758,#9759,#9760,
#9761,#9762,#9763,#9764,#9765,#9766,#9767,#9768,#9769,#9770,#9771,#9772,
#9773,#9774,#9775,#9776),.UNSPECIFIED.,.F.,.F.,(4,3,3,3,3,3,3,3,3,3,3,3,
3,3,3,3,3,3,3,3,3,3,3,4),(-0.411449009990747,-0.405504895608626,-0.398537948969837,
-0.388735121635006,-0.38221469543425,-0.375350878008265,-0.367728233026823,
-0.356236725744735,-0.347888396935362,-0.337683279819759,-0.326660059629232,
-0.31648347453161,-0.302658061144547,-0.289316835829758,-0.271192407431711,
-0.255261428895363,-0.2317752988163,-0.202135573454307,-0.16198628027259,
-0.126192133914446,-0.0754619856962401,-0.0360560096209726,-0.00196686147092064,
0.),.UNSPECIFIED.);
#127=B_SPLINE_CURVE_WITH_KNOTS('',5,(#9928,#9929,#9930,#9931,#9932,#9933,
#9934,#9935,#9936,#9937,#9938,#9939,#9940,#9941,#9942,#9943,#9944,#9945,
#9946,#9947,#9948,#9949,#9950,#9951,#9952,#9953,#9954,#9955,#9956,#9957,
#9958,#9959,#9960,#9961,#9962,#9963,#9964,#9965,#9966,#9967,#9968,#9969,
#9970,#9971,#9972,#9973,#9974,#9975,#9976,#9977,#9978,#9979,#9980,#9981,
#9982,#9983,#9984,#9985,#9986,#9987,#9988,#9989,#9990,#9991,#9992,#9993,
#9994,#9995,#9996,#9997,#9998,#9999,#10000,#10001),.UNSPECIFIED.,.F.,.F.,
(6,1,1,1,1,1,1,1,1,1,1,1,1,1,1,1,1,1,1,1,1,1,1,1,1,1,1,1,1,1,1,1,1,1,1,
1,1,1,1,1,1,1,1,1,1,1,1,1,1,1,1,1,1,1,1,1,1,1,1,1,1,1,1,1,1,1,1,1,1,6),
(0.,0.0142857142857143,0.0285714285714286,0.0428571428571429,0.0571428571428571,
0.0714285714285714,0.0857142857142857,0.1,0.114285714285714,0.128571428571429,
0.142857142857143,0.157142857142857,0.171428571428571,0.185714285714286,
0.2,0.214285714285714,0.228571428571429,0.242857142857143,0.257142857142857,
0.271428571428571,0.285714285714286,0.3,0.314285714285714,0.328571428571429,
0.342857142857143,0.357142857142857,0.371428571428571,0.385714285714286,
0.4,0.414285714285714,0.428571428571429,0.442857142857143,0.457142857142857,
0.471428571428572,0.485714285714286,0.5,0.514285714285714,0.528571428571429,
0.542857142857143,0.557142857142857,0.571428571428571,0.585714285714286,
0.6,0.614285714285714,0.628571428571428,0.642857142857142,0.657142857142857,
0.671428571428571,0.685714285714285,0.699999999999999,0.714285714285714,
0.728571428571428,0.742857142857142,0.757142857142856,0.771428571428571,
0.785714285714285,0.799999999999999,0.814285714285713,0.828571428571428,
0.842857142857142,0.857142857142856,0.87142857142857,0.885714285714284,
0.899999999999999,0.914285714285713,0.928571428571427,0.942857142857141,
0.957142857142856,0.97142857142857,1.),.UNSPECIFIED.);
#128=B_SPLINE_CURVE_WITH_KNOTS('',3,(#10003,#10004,#10005,#10006,#10007,
#10008,#10009,#10010,#10011,#10012,#10013,#10014,#10015,#10016,#10017,#10018,
#10019,#10020,#10021,#10022,#10023,#10024,#10025,#10026,#10027,#10028,#10029,
#10030,#10031,#10032,#10033,#10034,#10035,#10036,#10037,#10038,#10039,#10040,
#10041,#10042,#10043,#10044,#10045,#10046,#10047,#10048,#10049,#10050,#10051,
#10052,#10053,#10054,#10055,#10056,#10057,#10058,#10059,#10060,#10061,#10062,
#10063,#10064,#10065,#10066,#10067,#10068,#10069),.UNSPECIFIED.,.F.,.F.,
(4,3,3,3,3,3,3,3,3,3,3,3,3,3,3,3,3,3,3,3,3,3,4),(-0.0308474254187031,-0.028244314224116,
-0.0239308459820195,-0.020615261356278,-0.0170461143857998,-0.0150701376654228,
-0.0131660090191134,-0.0115202578917242,-0.0103391767722299,-0.00917732807803008,
-0.00816993700645051,-0.00725747183186186,-0.00648885936554755,-0.00537659349257577,
-0.0047045193060038,-0.00408467783901597,-0.00323202308941783,-0.00269108370365142,
-0.00220561578349396,-0.00169529231275093,-0.000847646156375465,-0.000380223898800284,
0.),.UNSPECIFIED.);
#129=B_SPLINE_CURVE_WITH_KNOTS('',5,(#10227,#10228,#10229,#10230,#10231,
#10232,#10233,#10234,#10235,#10236,#10237,#10238,#10239,#10240,#10241,#10242,
#10243,#10244,#10245,#10246,#10247,#10248,#10249,#10250,#10251,#10252,#10253,
#10254,#10255,#10256,#10257,#10258,#10259,#10260,#10261,#10262,#10263,#10264,
#10265,#10266,#10267,#10268,#10269,#10270,#10271,#10272,#10273,#10274,#10275,
#10276,#10277,#10278,#10279,#10280,#10281,#10282,#10283,#10284,#10285,#10286,
#10287,#10288,#10289,#10290,#10291,#10292,#10293,#10294,#10295,#10296,#10297,
#10298,#10299,#10300),.UNSPECIFIED.,.F.,.F.,(6,1,1,1,1,1,1,1,1,1,1,1,1,
1,1,1,1,1,1,1,1,1,1,1,1,1,1,1,1,1,1,1,1,1,1,1,1,1,1,1,1,1,1,1,1,1,1,1,1,
1,1,1,1,1,1,1,1,1,1,1,1,1,1,1,1,1,1,1,1,6),(0.,0.0142857142857143,0.0285714285714286,
0.0428571428571429,0.0571428571428571,0.0714285714285714,0.0857142857142857,
0.1,0.114285714285714,0.128571428571429,0.142857142857143,0.157142857142857,
0.171428571428571,0.185714285714286,0.2,0.214285714285714,0.228571428571429,
0.242857142857143,0.257142857142857,0.271428571428571,0.285714285714286,
0.3,0.314285714285714,0.328571428571429,0.342857142857143,0.357142857142857,
0.371428571428571,0.385714285714286,0.4,0.414285714285714,0.428571428571429,
0.442857142857143,0.457142857142857,0.471428571428572,0.485714285714286,
0.5,0.514285714285714,0.528571428571429,0.542857142857143,0.557142857142857,
0.571428571428571,0.585714285714286,0.6,0.614285714285714,0.628571428571428,
0.642857142857142,0.657142857142857,0.671428571428571,0.685714285714285,
0.699999999999999,0.714285714285714,0.728571428571428,0.742857142857142,
0.757142857142856,0.771428571428571,0.785714285714285,0.799999999999999,
0.814285714285713,0.828571428571428,0.842857142857142,0.857142857142856,
0.87142857142857,0.885714285714284,0.899999999999999,0.914285714285713,
0.928571428571427,0.942857142857141,0.957142857142856,0.97142857142857,
1.),.UNSPECIFIED.);
#130=B_SPLINE_CURVE_WITH_KNOTS('',3,(#10301,#10302,#10303,#10304,#10305,
#10306,#10307,#10308,#10309,#10310,#10311,#10312,#10313,#10314,#10315,#10316,
#10317,#10318,#10319,#10320,#10321,#10322,#10323,#10324,#10325,#10326,#10327,
#10328,#10329,#10330,#10331,#10332,#10333,#10334,#10335,#10336,#10337,#10338,
#10339,#10340,#10341,#10342,#10343,#10344,#10345,#10346,#10347,#10348,#10349,
#10350,#10351,#10352,#10353,#10354,#10355,#10356,#10357,#10358,#10359,#10360,
#10361,#10362,#10363,#10364,#10365,#10366,#10367,#10368,#10369,#10370),
 .UNSPECIFIED.,.F.,.F.,(4,3,3,3,3,3,3,3,3,3,3,3,3,3,3,3,3,3,3,3,3,3,3,4),
(-0.411449009784292,-0.405504895410621,-0.398537948775868,-0.388735121437593,
-0.382214695240303,-0.375350877816651,-0.367728232839072,-0.356236725562851,
-0.347888396756906,-0.33768327964519,-0.326660059462181,-0.31648347436891,
-0.302658061000279,-0.289316835703338,-0.271192407317085,-0.255261428783421,
-0.231775298711656,-0.20213557335682,-0.161986280248108,-0.126192134001441,
-0.0754619855590316,-0.036056011065119,-0.00196686534552455,0.),
 .UNSPECIFIED.);
#131=B_SPLINE_CURVE_WITH_KNOTS('',5,(#10522,#10523,#10524,#10525,#10526,
#10527,#10528,#10529,#10530,#10531,#10532,#10533,#10534,#10535,#10536,#10537,
#10538,#10539,#10540,#10541,#10542,#10543,#10544,#10545,#10546,#10547,#10548,
#10549,#10550,#10551,#10552,#10553,#10554,#10555,#10556,#10557,#10558,#10559,
#10560,#10561,#10562,#10563,#10564,#10565,#10566,#10567,#10568,#10569,#10570,
#10571,#10572,#10573,#10574,#10575,#10576,#10577,#10578,#10579,#10580,#10581,
#10582,#10583,#10584,#10585,#10586,#10587,#10588,#10589,#10590,#10591,#10592,
#10593,#10594,#10595),.UNSPECIFIED.,.F.,.F.,(6,1,1,1,1,1,1,1,1,1,1,1,1,
1,1,1,1,1,1,1,1,1,1,1,1,1,1,1,1,1,1,1,1,1,1,1,1,1,1,1,1,1,1,1,1,1,1,1,1,
1,1,1,1,1,1,1,1,1,1,1,1,1,1,1,1,1,1,1,1,6),(0.,0.0142857142857143,0.0285714285714286,
0.0428571428571429,0.0571428571428571,0.0714285714285714,0.0857142857142857,
0.1,0.114285714285714,0.128571428571429,0.142857142857143,0.157142857142857,
0.171428571428571,0.185714285714286,0.2,0.214285714285714,0.228571428571429,
0.242857142857143,0.257142857142857,0.271428571428571,0.285714285714286,
0.3,0.314285714285714,0.328571428571429,0.342857142857143,0.357142857142857,
0.371428571428571,0.385714285714286,0.4,0.414285714285714,0.428571428571429,
0.442857142857143,0.457142857142857,0.471428571428572,0.485714285714286,
0.5,0.514285714285714,0.528571428571429,0.542857142857143,0.557142857142857,
0.571428571428571,0.585714285714286,0.6,0.614285714285714,0.628571428571428,
0.642857142857142,0.657142857142857,0.671428571428571,0.685714285714285,
0.699999999999999,0.714285714285714,0.728571428571428,0.742857142857142,
0.757142857142856,0.771428571428571,0.785714285714285,0.799999999999999,
0.814285714285713,0.828571428571428,0.842857142857142,0.857142857142856,
0.87142857142857,0.885714285714284,0.899999999999999,0.914285714285713,
0.928571428571427,0.942857142857141,0.957142857142856,0.97142857142857,
1.),.UNSPECIFIED.);
#132=B_SPLINE_CURVE_WITH_KNOTS('',3,(#10597,#10598,#10599,#10600,#10601,
#10602,#10603,#10604,#10605,#10606,#10607,#10608,#10609,#10610,#10611,#10612,
#10613,#10614,#10615,#10616,#10617,#10618,#10619,#10620,#10621,#10622,#10623,
#10624,#10625,#10626,#10627,#10628,#10629,#10630,#10631,#10632,#10633,#10634,
#10635,#10636,#10637,#10638,#10639,#10640,#10641,#10642,#10643,#10644,#10645,
#10646,#10647,#10648,#10649,#10650,#10651,#10652,#10653,#10654,#10655,#10656,
#10657,#10658,#10659,#10660,#10661,#10662,#10663),.UNSPECIFIED.,.F.,.F.,
(4,3,3,3,3,3,3,3,3,3,3,3,3,3,3,3,3,3,3,3,3,3,4),(-0.0308474254321917,-0.0282443140955979,
-0.0239308458396743,-0.020615261220034,-0.0170461143578005,-0.0150701375986627,
-0.0131660090560162,-0.0115202579240142,-0.0103391768048034,-0.00917732809651329,
-0.00816993701567056,-0.00725747184422916,-0.00648885937671962,-0.00537659348714137,
-0.0047045193012487,-0.00408467783345363,-0.00323202309358667,-0.00269108370723003,
-0.00220561578671065,-0.00169529231611998,-0.000847646158059989,-0.000380223899959456,
0.),.UNSPECIFIED.);
#133=B_SPLINE_CURVE_WITH_KNOTS('',5,(#10821,#10822,#10823,#10824,#10825,
#10826,#10827,#10828,#10829,#10830,#10831,#10832,#10833,#10834,#10835,#10836,
#10837,#10838,#10839,#10840,#10841,#10842,#10843,#10844,#10845,#10846,#10847,
#10848,#10849,#10850,#10851,#10852,#10853,#10854,#10855,#10856,#10857,#10858,
#10859,#10860,#10861,#10862,#10863,#10864,#10865,#10866,#10867,#10868,#10869,
#10870,#10871,#10872,#10873,#10874,#10875,#10876,#10877,#10878,#10879,#10880,
#10881,#10882,#10883,#10884,#10885,#10886,#10887,#10888,#10889,#10890,#10891,
#10892,#10893,#10894),.UNSPECIFIED.,.F.,.F.,(6,1,1,1,1,1,1,1,1,1,1,1,1,
1,1,1,1,1,1,1,1,1,1,1,1,1,1,1,1,1,1,1,1,1,1,1,1,1,1,1,1,1,1,1,1,1,1,1,1,
1,1,1,1,1,1,1,1,1,1,1,1,1,1,1,1,1,1,1,1,6),(0.,0.0142857142857143,0.0285714285714286,
0.0428571428571429,0.0571428571428571,0.0714285714285714,0.0857142857142857,
0.1,0.114285714285714,0.128571428571429,0.142857142857143,0.157142857142857,
0.171428571428571,0.185714285714286,0.2,0.214285714285714,0.228571428571429,
0.242857142857143,0.257142857142857,0.271428571428571,0.285714285714286,
0.3,0.314285714285714,0.328571428571429,0.342857142857143,0.357142857142857,
0.371428571428571,0.385714285714286,0.4,0.414285714285714,0.428571428571429,
0.442857142857143,0.457142857142857,0.471428571428572,0.485714285714286,
0.5,0.514285714285714,0.528571428571429,0.542857142857143,0.557142857142857,
0.571428571428571,0.585714285714286,0.6,0.614285714285714,0.628571428571428,
0.642857142857142,0.657142857142857,0.671428571428571,0.685714285714285,
0.699999999999999,0.714285714285714,0.728571428571428,0.742857142857142,
0.757142857142856,0.771428571428571,0.785714285714285,0.799999999999999,
0.814285714285713,0.828571428571428,0.842857142857142,0.857142857142856,
0.87142857142857,0.885714285714284,0.899999999999999,0.914285714285713,
0.928571428571427,0.942857142857141,0.957142857142856,0.97142857142857,
1.),.UNSPECIFIED.);
#134=B_SPLINE_CURVE_WITH_KNOTS('',3,(#10895,#10896,#10897,#10898,#10899,
#10900,#10901,#10902,#10903,#10904,#10905,#10906,#10907,#10908,#10909,#10910,
#10911,#10912,#10913,#10914,#10915,#10916,#10917,#10918,#10919,#10920,#10921,
#10922,#10923,#10924,#10925,#10926,#10927,#10928,#10929,#10930,#10931,#10932,
#10933,#10934,#10935,#10936,#10937,#10938,#10939,#10940,#10941,#10942,#10943,
#10944,#10945,#10946,#10947,#10948,#10949,#10950,#10951,#10952,#10953,#10954,
#10955,#10956,#10957,#10958,#10959,#10960,#10961,#10962,#10963,#10964),
 .UNSPECIFIED.,.F.,.F.,(4,3,3,3,3,3,3,3,3,3,3,3,3,3,3,3,3,3,3,3,3,3,3,4),
(-0.41144900970185,-0.405504895343942,-0.398537948713814,-0.388735121356617,
-0.382214695160452,-0.375350877738258,-0.367728232762158,-0.356236725488341,
-0.34788839668605,-0.33768327957583,-0.326660059396151,-0.316483474305328,
-0.302658060948649,-0.289316835657715,-0.271192407308052,-0.255261428784221,
-0.231775298718215,-0.202135573387617,-0.16198628027827,-0.126192134079699,
-0.0754619858625935,-0.0360560120089752,-0.00196686783518586,0.),
 .UNSPECIFIED.);
#135=B_SPLINE_CURVE_WITH_KNOTS('',5,(#11116,#11117,#11118,#11119,#11120,
#11121,#11122,#11123,#11124,#11125,#11126,#11127,#11128,#11129,#11130,#11131,
#11132,#11133,#11134,#11135,#11136,#11137,#11138,#11139,#11140,#11141,#11142,
#11143,#11144,#11145,#11146,#11147,#11148,#11149,#11150,#11151,#11152,#11153,
#11154,#11155,#11156,#11157,#11158,#11159,#11160,#11161,#11162,#11163,#11164,
#11165,#11166,#11167,#11168,#11169,#11170,#11171,#11172,#11173,#11174,#11175,
#11176,#11177,#11178,#11179,#11180,#11181,#11182,#11183,#11184,#11185,#11186,
#11187,#11188,#11189),.UNSPECIFIED.,.F.,.F.,(6,1,1,1,1,1,1,1,1,1,1,1,1,
1,1,1,1,1,1,1,1,1,1,1,1,1,1,1,1,1,1,1,1,1,1,1,1,1,1,1,1,1,1,1,1,1,1,1,1,
1,1,1,1,1,1,1,1,1,1,1,1,1,1,1,1,1,1,1,1,6),(0.,0.0142857142857143,0.0285714285714286,
0.0428571428571429,0.0571428571428571,0.0714285714285714,0.0857142857142857,
0.1,0.114285714285714,0.128571428571429,0.142857142857143,0.157142857142857,
0.171428571428571,0.185714285714286,0.2,0.214285714285714,0.228571428571429,
0.242857142857143,0.257142857142857,0.271428571428571,0.285714285714286,
0.3,0.314285714285714,0.328571428571429,0.342857142857143,0.357142857142857,
0.371428571428571,0.385714285714286,0.4,0.414285714285714,0.428571428571429,
0.442857142857143,0.457142857142857,0.471428571428572,0.485714285714286,
0.5,0.514285714285714,0.528571428571429,0.542857142857143,0.557142857142857,
0.571428571428571,0.585714285714286,0.6,0.614285714285714,0.628571428571428,
0.642857142857142,0.657142857142857,0.671428571428571,0.685714285714285,
0.699999999999999,0.714285714285714,0.728571428571428,0.742857142857142,
0.757142857142856,0.771428571428571,0.785714285714285,0.799999999999999,
0.814285714285713,0.828571428571428,0.842857142857142,0.857142857142856,
0.87142857142857,0.885714285714284,0.899999999999999,0.914285714285713,
0.928571428571427,0.942857142857141,0.957142857142856,0.97142857142857,
1.),.UNSPECIFIED.);
#136=B_SPLINE_CURVE_WITH_KNOTS('',3,(#11191,#11192,#11193,#11194,#11195,
#11196,#11197,#11198,#11199,#11200,#11201,#11202,#11203,#11204,#11205,#11206,
#11207,#11208,#11209,#11210,#11211,#11212,#11213,#11214,#11215,#11216,#11217,
#11218,#11219,#11220,#11221,#11222,#11223,#11224,#11225,#11226,#11227,#11228,
#11229,#11230,#11231,#11232,#11233,#11234,#11235,#11236,#11237,#11238,#11239,
#11240,#11241,#11242,#11243,#11244,#11245,#11246,#11247,#11248,#11249,#11250,
#11251,#11252,#11253,#11254,#11255,#11256,#11257),.UNSPECIFIED.,.F.,.F.,
(4,3,3,3,3,3,3,3,3,3,3,3,3,3,3,3,3,3,3,3,3,3,4),(-0.0308474254313729,-0.0282443144331512,
-0.0239308462436385,-0.0206152616062002,-0.017046114491142,-0.0150701378789916,
-0.0131660089309141,-0.0115202578145499,-0.0103391766904584,-0.0091773280428693,
-0.00816993699591886,-0.00725747180427489,-0.00648885934148822,-0.00537659351838039,
-0.00470451932858284,-0.00408467786302119,-0.00323202308259216,-0.00269108369773592,
-0.00220561577775678,-0.00169529230541892,-0.00084764615270946,-0.000380223895080282,
0.),.UNSPECIFIED.);
#137=B_SPLINE_CURVE_WITH_KNOTS('',5,(#11415,#11416,#11417,#11418,#11419,
#11420,#11421,#11422,#11423,#11424,#11425,#11426,#11427,#11428,#11429,#11430,
#11431,#11432,#11433,#11434,#11435,#11436,#11437,#11438,#11439,#11440,#11441,
#11442,#11443,#11444,#11445,#11446,#11447,#11448,#11449,#11450,#11451,#11452,
#11453,#11454,#11455,#11456,#11457,#11458,#11459,#11460,#11461,#11462,#11463,
#11464,#11465,#11466,#11467,#11468,#11469,#11470,#11471,#11472,#11473,#11474,
#11475,#11476,#11477,#11478,#11479,#11480,#11481,#11482,#11483,#11484,#11485,
#11486,#11487,#11488),.UNSPECIFIED.,.F.,.F.,(6,1,1,1,1,1,1,1,1,1,1,1,1,
1,1,1,1,1,1,1,1,1,1,1,1,1,1,1,1,1,1,1,1,1,1,1,1,1,1,1,1,1,1,1,1,1,1,1,1,
1,1,1,1,1,1,1,1,1,1,1,1,1,1,1,1,1,1,1,1,6),(0.,0.0142857142857143,0.0285714285714286,
0.0428571428571429,0.0571428571428571,0.0714285714285714,0.0857142857142857,
0.1,0.114285714285714,0.128571428571429,0.142857142857143,0.157142857142857,
0.171428571428571,0.185714285714286,0.2,0.214285714285714,0.228571428571429,
0.242857142857143,0.257142857142857,0.271428571428571,0.285714285714286,
0.3,0.314285714285714,0.328571428571429,0.342857142857143,0.357142857142857,
0.371428571428571,0.385714285714286,0.4,0.414285714285714,0.428571428571429,
0.442857142857143,0.457142857142857,0.471428571428572,0.485714285714286,
0.5,0.514285714285714,0.528571428571429,0.542857142857143,0.557142857142857,
0.571428571428571,0.585714285714286,0.6,0.614285714285714,0.628571428571428,
0.642857142857142,0.657142857142857,0.671428571428571,0.685714285714285,
0.699999999999999,0.714285714285714,0.728571428571428,0.742857142857142,
0.757142857142856,0.771428571428571,0.785714285714285,0.799999999999999,
0.814285714285713,0.828571428571428,0.842857142857142,0.857142857142856,
0.87142857142857,0.885714285714284,0.899999999999999,0.914285714285713,
0.928571428571427,0.942857142857141,0.957142857142856,0.97142857142857,
1.),.UNSPECIFIED.);
#138=B_SPLINE_CURVE_WITH_KNOTS('',3,(#11489,#11490,#11491,#11492,#11493,
#11494,#11495,#11496,#11497,#11498,#11499,#11500,#11501,#11502,#11503,#11504,
#11505,#11506,#11507,#11508,#11509,#11510,#11511,#11512,#11513,#11514,#11515,
#11516,#11517,#11518,#11519,#11520,#11521,#11522,#11523,#11524,#11525,#11526,
#11527,#11528,#11529,#11530,#11531,#11532,#11533,#11534,#11535,#11536,#11537,
#11538,#11539,#11540,#11541,#11542,#11543,#11544,#11545,#11546,#11547,#11548,
#11549,#11550,#11551,#11552,#11553,#11554,#11555,#11556,#11557,#11558),
 .UNSPECIFIED.,.F.,.F.,(4,3,3,3,3,3,3,3,3,3,3,3,3,3,3,3,3,3,3,3,3,3,3,4),
(-0.411449009745582,-0.405504895379435,-0.398537948745384,-0.388735121403136,
-0.382214695205601,-0.375350877782795,-0.367728232806823,-0.35623672553161,
-0.347888396726707,-0.337683279620391,-0.326660059439279,-0.316483474349347,
-0.302658060997721,-0.289316835702375,-0.271192407460765,-0.255261428951979,
-0.231775298732412,-0.202135573328733,-0.161986280135987,-0.12619213402364,
-0.0754619855322879,-0.0360560073833462,-0.00196685495466459,0.),
 .UNSPECIFIED.);
#139=B_SPLINE_CURVE_WITH_KNOTS('',5,(#11710,#11711,#11712,#11713,#11714,
#11715,#11716,#11717,#11718,#11719,#11720,#11721,#11722,#11723,#11724,#11725,
#11726,#11727,#11728,#11729,#11730,#11731,#11732,#11733,#11734,#11735,#11736,
#11737,#11738,#11739,#11740,#11741,#11742,#11743,#11744,#11745,#11746,#11747,
#11748,#11749,#11750,#11751,#11752,#11753,#11754,#11755,#11756,#11757,#11758,
#11759,#11760,#11761,#11762,#11763,#11764,#11765,#11766,#11767,#11768,#11769,
#11770,#11771,#11772,#11773,#11774,#11775,#11776,#11777,#11778,#11779,#11780,
#11781,#11782,#11783),.UNSPECIFIED.,.F.,.F.,(6,1,1,1,1,1,1,1,1,1,1,1,1,
1,1,1,1,1,1,1,1,1,1,1,1,1,1,1,1,1,1,1,1,1,1,1,1,1,1,1,1,1,1,1,1,1,1,1,1,
1,1,1,1,1,1,1,1,1,1,1,1,1,1,1,1,1,1,1,1,6),(0.,0.0142857142857143,0.0285714285714286,
0.0428571428571429,0.0571428571428571,0.0714285714285714,0.0857142857142857,
0.1,0.114285714285714,0.128571428571429,0.142857142857143,0.157142857142857,
0.171428571428571,0.185714285714286,0.2,0.214285714285714,0.228571428571429,
0.242857142857143,0.257142857142857,0.271428571428571,0.285714285714286,
0.3,0.314285714285714,0.328571428571429,0.342857142857143,0.357142857142857,
0.371428571428571,0.385714285714286,0.4,0.414285714285714,0.428571428571429,
0.442857142857143,0.457142857142857,0.471428571428572,0.485714285714286,
0.5,0.514285714285714,0.528571428571429,0.542857142857143,0.557142857142857,
0.571428571428571,0.585714285714286,0.6,0.614285714285714,0.628571428571428,
0.642857142857142,0.657142857142857,0.671428571428571,0.685714285714285,
0.699999999999999,0.714285714285714,0.728571428571428,0.742857142857142,
0.757142857142856,0.771428571428571,0.785714285714285,0.799999999999999,
0.814285714285713,0.828571428571428,0.842857142857142,0.857142857142856,
0.87142857142857,0.885714285714284,0.899999999999999,0.914285714285713,
0.928571428571427,0.942857142857141,0.957142857142856,0.97142857142857,
1.),.UNSPECIFIED.);
#140=B_SPLINE_CURVE_WITH_KNOTS('',3,(#11785,#11786,#11787,#11788,#11789,
#11790,#11791,#11792,#11793,#11794,#11795,#11796,#11797,#11798,#11799,#11800,
#11801,#11802,#11803,#11804,#11805,#11806,#11807,#11808,#11809,#11810,#11811,
#11812,#11813,#11814,#11815,#11816,#11817,#11818,#11819,#11820,#11821,#11822,
#11823,#11824,#11825,#11826,#11827,#11828,#11829,#11830,#11831,#11832,#11833,
#11834,#11835,#11836,#11837,#11838,#11839,#11840,#11841,#11842,#11843,#11844,
#11845,#11846,#11847,#11848,#11849,#11850,#11851),.UNSPECIFIED.,.F.,.F.,
(4,3,3,3,3,3,3,3,3,3,3,3,3,3,3,3,3,3,3,3,3,3,4),(-0.0308474254096501,-0.028244313899376,
-0.0239308455956517,-0.020615260955671,-0.0170461143005811,-0.0150701375011353,
-0.0131660090769615,-0.0115202579423413,-0.0103391768283886,-0.00917732810453088,
-0.0081699370150875,-0.00725747185097503,-0.0064888593825484,-0.00537659347407927,
-0.00470451928981936,-0.00408467782188743,-0.00323202309462087,-0.00269108370824936,
-0.00220561578794048,-0.00169529231835461,-0.000847646159177307,-0.000380223901533956,
0.),.UNSPECIFIED.);
#141=B_SPLINE_CURVE_WITH_KNOTS('',5,(#12009,#12010,#12011,#12012,#12013,
#12014,#12015,#12016,#12017,#12018,#12019,#12020,#12021,#12022,#12023,#12024,
#12025,#12026,#12027,#12028,#12029,#12030,#12031,#12032,#12033,#12034,#12035,
#12036,#12037,#12038,#12039,#12040,#12041,#12042,#12043,#12044,#12045,#12046,
#12047,#12048,#12049,#12050,#12051,#12052,#12053,#12054,#12055,#12056,#12057,
#12058,#12059,#12060,#12061,#12062,#12063,#12064,#12065,#12066,#12067,#12068,
#12069,#12070,#12071,#12072,#12073,#12074,#12075,#12076,#12077,#12078,#12079,
#12080,#12081,#12082),.UNSPECIFIED.,.F.,.F.,(6,1,1,1,1,1,1,1,1,1,1,1,1,
1,1,1,1,1,1,1,1,1,1,1,1,1,1,1,1,1,1,1,1,1,1,1,1,1,1,1,1,1,1,1,1,1,1,1,1,
1,1,1,1,1,1,1,1,1,1,1,1,1,1,1,1,1,1,1,1,6),(0.,0.0142857142857143,0.0285714285714286,
0.0428571428571429,0.0571428571428571,0.0714285714285714,0.0857142857142857,
0.1,0.114285714285714,0.128571428571429,0.142857142857143,0.157142857142857,
0.171428571428571,0.185714285714286,0.2,0.214285714285714,0.228571428571429,
0.242857142857143,0.257142857142857,0.271428571428571,0.285714285714286,
0.3,0.314285714285714,0.328571428571429,0.342857142857143,0.357142857142857,
0.371428571428571,0.385714285714286,0.4,0.414285714285714,0.428571428571429,
0.442857142857143,0.457142857142857,0.471428571428572,0.485714285714286,
0.5,0.514285714285714,0.528571428571429,0.542857142857143,0.557142857142857,
0.571428571428571,0.585714285714286,0.6,0.614285714285714,0.628571428571428,
0.642857142857142,0.657142857142857,0.671428571428571,0.685714285714285,
0.699999999999999,0.714285714285714,0.728571428571428,0.742857142857142,
0.757142857142856,0.771428571428571,0.785714285714285,0.799999999999999,
0.814285714285713,0.828571428571428,0.842857142857142,0.857142857142856,
0.87142857142857,0.885714285714284,0.899999999999999,0.914285714285713,
0.928571428571427,0.942857142857141,0.957142857142856,0.97142857142857,
1.),.UNSPECIFIED.);
#142=B_SPLINE_CURVE_WITH_KNOTS('',3,(#12083,#12084,#12085,#12086,#12087,
#12088,#12089,#12090,#12091,#12092,#12093,#12094,#12095,#12096,#12097,#12098,
#12099,#12100,#12101,#12102,#12103,#12104,#12105,#12106,#12107,#12108,#12109,
#12110,#12111,#12112,#12113,#12114,#12115,#12116,#12117,#12118,#12119,#12120,
#12121,#12122,#12123,#12124,#12125,#12126,#12127,#12128,#12129,#12130,#12131,
#12132,#12133,#12134,#12135,#12136,#12137,#12138,#12139,#12140,#12141,#12142,
#12143,#12144,#12145,#12146,#12147,#12148,#12149,#12150,#12151,#12152),
 .UNSPECIFIED.,.F.,.F.,(4,3,3,3,3,3,3,3,3,3,3,3,3,3,3,3,3,3,3,3,3,3,3,4),
(-0.411449009865562,-0.4055048954869,-0.398537948850747,-0.388735121518256,
-0.382214695319647,-0.375350877895016,-0.3677282329171,-0.35623672563844,
-0.347888396831227,-0.337683279715536,-0.326660059528631,-0.316483474438613,
-0.302658061094389,-0.28931683580642,-0.271192407552387,-0.255261429122638,
-0.231775298922887,-0.202135573548005,-0.161986280573123,-0.126192134261937,
-0.0754619859222758,-0.0360560139042322,-0.00196687400591684,0.),
 .UNSPECIFIED.);
#143=B_SPLINE_CURVE_WITH_KNOTS('',5,(#12304,#12305,#12306,#12307,#12308,
#12309,#12310,#12311,#12312,#12313,#12314,#12315,#12316,#12317,#12318,#12319,
#12320,#12321,#12322,#12323,#12324,#12325,#12326,#12327,#12328,#12329,#12330,
#12331,#12332,#12333,#12334,#12335,#12336,#12337,#12338,#12339,#12340,#12341,
#12342,#12343,#12344,#12345,#12346,#12347,#12348,#12349,#12350,#12351,#12352,
#12353,#12354,#12355,#12356,#12357,#12358,#12359,#12360,#12361,#12362,#12363,
#12364,#12365,#12366,#12367,#12368,#12369,#12370,#12371,#12372,#12373,#12374,
#12375,#12376,#12377),.UNSPECIFIED.,.F.,.F.,(6,1,1,1,1,1,1,1,1,1,1,1,1,
1,1,1,1,1,1,1,1,1,1,1,1,1,1,1,1,1,1,1,1,1,1,1,1,1,1,1,1,1,1,1,1,1,1,1,1,
1,1,1,1,1,1,1,1,1,1,1,1,1,1,1,1,1,1,1,1,6),(0.,0.0142857142857143,0.0285714285714286,
0.0428571428571429,0.0571428571428571,0.0714285714285714,0.0857142857142857,
0.1,0.114285714285714,0.128571428571429,0.142857142857143,0.157142857142857,
0.171428571428571,0.185714285714286,0.2,0.214285714285714,0.228571428571429,
0.242857142857143,0.257142857142857,0.271428571428571,0.285714285714286,
0.3,0.314285714285714,0.328571428571429,0.342857142857143,0.357142857142857,
0.371428571428571,0.385714285714286,0.4,0.414285714285714,0.428571428571429,
0.442857142857143,0.457142857142857,0.471428571428572,0.485714285714286,
0.5,0.514285714285714,0.528571428571429,0.542857142857143,0.557142857142857,
0.571428571428571,0.585714285714286,0.6,0.614285714285714,0.628571428571428,
0.642857142857142,0.657142857142857,0.671428571428571,0.685714285714285,
0.699999999999999,0.714285714285714,0.728571428571428,0.742857142857142,
0.757142857142856,0.771428571428571,0.785714285714285,0.799999999999999,
0.814285714285713,0.828571428571428,0.842857142857142,0.857142857142856,
0.87142857142857,0.885714285714284,0.899999999999999,0.914285714285713,
0.928571428571427,0.942857142857141,0.957142857142856,0.97142857142857,
1.),.UNSPECIFIED.);
#144=B_SPLINE_CURVE_WITH_KNOTS('',3,(#12379,#12380,#12381,#12382,#12383,
#12384,#12385,#12386,#12387,#12388,#12389,#12390,#12391,#12392,#12393,#12394,
#12395,#12396,#12397,#12398,#12399,#12400,#12401,#12402,#12403,#12404,#12405,
#12406,#12407,#12408,#12409,#12410,#12411,#12412,#12413,#12414,#12415,#12416,
#12417,#12418,#12419,#12420,#12421,#12422,#12423,#12424,#12425,#12426,#12427,
#12428,#12429,#12430,#12431,#12432,#12433,#12434,#12435,#12436,#12437,#12438,
#12439,#12440,#12441,#12442,#12443,#12444,#12445),.UNSPECIFIED.,.F.,.F.,
(4,3,3,3,3,3,3,3,3,3,3,3,3,3,3,3,3,3,3,3,3,3,4),(-0.0308474254198399,-0.0282443142846492,
-0.0239308460906392,-0.0206152614646765,-0.0170461144159942,-0.0150701377147652,
-0.0131660089970923,-0.0115202578724558,-0.0103391767515509,-0.00917732806988761,
-0.00816993700370822,-0.00725747182636578,-0.00648885936066672,-0.00537659349685568,
-0.00470451930974872,-0.00408467784315956,-0.00323202308807464,-0.00269108370254087,
-0.00220561578241539,-0.00169529231143548,-0.000847646155717738,-0.000380223898423687,
0.),.UNSPECIFIED.);
#145=B_SPLINE_CURVE_WITH_KNOTS('',5,(#12603,#12604,#12605,#12606,#12607,
#12608,#12609,#12610,#12611,#12612,#12613,#12614,#12615,#12616,#12617,#12618,
#12619,#12620,#12621,#12622,#12623,#12624,#12625,#12626,#12627,#12628,#12629,
#12630,#12631,#12632,#12633,#12634,#12635,#12636,#12637,#12638,#12639,#12640,
#12641,#12642,#12643,#12644,#12645,#12646,#12647,#12648,#12649,#12650,#12651,
#12652,#12653,#12654,#12655,#12656,#12657,#12658,#12659,#12660,#12661,#12662,
#12663,#12664,#12665,#12666,#12667,#12668,#12669,#12670,#12671,#12672,#12673,
#12674,#12675,#12676),.UNSPECIFIED.,.F.,.F.,(6,1,1,1,1,1,1,1,1,1,1,1,1,
1,1,1,1,1,1,1,1,1,1,1,1,1,1,1,1,1,1,1,1,1,1,1,1,1,1,1,1,1,1,1,1,1,1,1,1,
1,1,1,1,1,1,1,1,1,1,1,1,1,1,1,1,1,1,1,1,6),(0.,0.0142857142857143,0.0285714285714286,
0.0428571428571429,0.0571428571428571,0.0714285714285714,0.0857142857142857,
0.1,0.114285714285714,0.128571428571429,0.142857142857143,0.157142857142857,
0.171428571428571,0.185714285714286,0.2,0.214285714285714,0.228571428571429,
0.242857142857143,0.257142857142857,0.271428571428571,0.285714285714286,
0.3,0.314285714285714,0.328571428571429,0.342857142857143,0.357142857142857,
0.371428571428571,0.385714285714286,0.4,0.414285714285714,0.428571428571429,
0.442857142857143,0.457142857142857,0.471428571428572,0.485714285714286,
0.5,0.514285714285714,0.528571428571429,0.542857142857143,0.557142857142857,
0.571428571428571,0.585714285714286,0.6,0.614285714285714,0.628571428571428,
0.642857142857142,0.657142857142857,0.671428571428571,0.685714285714285,
0.699999999999999,0.714285714285714,0.728571428571428,0.742857142857142,
0.757142857142856,0.771428571428571,0.785714285714285,0.799999999999999,
0.814285714285713,0.828571428571428,0.842857142857142,0.857142857142856,
0.87142857142857,0.885714285714284,0.899999999999999,0.914285714285713,
0.928571428571427,0.942857142857141,0.957142857142856,0.97142857142857,
1.),.UNSPECIFIED.);
#146=B_SPLINE_CURVE_WITH_KNOTS('',3,(#12677,#12678,#12679,#12680,#12681,
#12682,#12683,#12684,#12685,#12686,#12687,#12688,#12689,#12690,#12691,#12692,
#12693,#12694,#12695,#12696,#12697,#12698,#12699,#12700,#12701,#12702,#12703,
#12704,#12705,#12706,#12707,#12708,#12709,#12710,#12711,#12712,#12713,#12714,
#12715,#12716,#12717,#12718,#12719,#12720,#12721,#12722,#12723,#12724,#12725,
#12726,#12727,#12728,#12729,#12730,#12731,#12732,#12733,#12734,#12735,#12736,
#12737,#12738,#12739,#12740,#12741,#12742,#12743,#12744,#12745,#12746),
 .UNSPECIFIED.,.F.,.F.,(4,3,3,3,3,3,3,3,3,3,3,3,3,3,3,3,3,3,3,3,3,3,3,4),
(-0.411449010137647,-0.405504895753404,-0.398537949112127,-0.388735121773796,
-0.382214695570712,-0.375350878142277,-0.367728233158118,-0.356236725871927,
-0.347888397059155,-0.337683279939957,-0.326660059745585,-0.316483474644296,
-0.302658061251899,-0.289316835931869,-0.271192407516363,-0.255261428973649,
-0.231775298903159,-0.202135573529554,-0.161986280339301,-0.126192134013684,
-0.0754619855442812,-0.0360560094852106,-0.00196686131918792,0.),
 .UNSPECIFIED.);
#147=B_SPLINE_CURVE_WITH_KNOTS('',5,(#12898,#12899,#12900,#12901,#12902,
#12903,#12904,#12905,#12906,#12907,#12908,#12909,#12910,#12911,#12912,#12913,
#12914,#12915,#12916,#12917,#12918,#12919,#12920,#12921,#12922,#12923,#12924,
#12925,#12926,#12927,#12928,#12929,#12930,#12931,#12932,#12933,#12934,#12935,
#12936,#12937,#12938,#12939,#12940,#12941,#12942,#12943,#12944,#12945,#12946,
#12947,#12948,#12949,#12950,#12951,#12952,#12953,#12954,#12955,#12956,#12957,
#12958,#12959,#12960,#12961,#12962,#12963,#12964,#12965,#12966,#12967,#12968,
#12969,#12970,#12971),.UNSPECIFIED.,.F.,.F.,(6,1,1,1,1,1,1,1,1,1,1,1,1,
1,1,1,1,1,1,1,1,1,1,1,1,1,1,1,1,1,1,1,1,1,1,1,1,1,1,1,1,1,1,1,1,1,1,1,1,
1,1,1,1,1,1,1,1,1,1,1,1,1,1,1,1,1,1,1,1,6),(0.,0.0142857142857143,0.0285714285714286,
0.0428571428571429,0.0571428571428571,0.0714285714285714,0.0857142857142857,
0.1,0.114285714285714,0.128571428571429,0.142857142857143,0.157142857142857,
0.171428571428571,0.185714285714286,0.2,0.214285714285714,0.228571428571429,
0.242857142857143,0.257142857142857,0.271428571428571,0.285714285714286,
0.3,0.314285714285714,0.328571428571429,0.342857142857143,0.357142857142857,
0.371428571428571,0.385714285714286,0.4,0.414285714285714,0.428571428571429,
0.442857142857143,0.457142857142857,0.471428571428572,0.485714285714286,
0.5,0.514285714285714,0.528571428571429,0.542857142857143,0.557142857142857,
0.571428571428571,0.585714285714286,0.6,0.614285714285714,0.628571428571428,
0.642857142857142,0.657142857142857,0.671428571428571,0.685714285714285,
0.699999999999999,0.714285714285714,0.728571428571428,0.742857142857142,
0.757142857142856,0.771428571428571,0.785714285714285,0.799999999999999,
0.814285714285713,0.828571428571428,0.842857142857142,0.857142857142856,
0.87142857142857,0.885714285714284,0.899999999999999,0.914285714285713,
0.928571428571427,0.942857142857141,0.957142857142856,0.97142857142857,
1.),.UNSPECIFIED.);
#148=B_SPLINE_CURVE_WITH_KNOTS('',3,(#12973,#12974,#12975,#12976,#12977,
#12978,#12979,#12980,#12981,#12982,#12983,#12984,#12985,#12986,#12987,#12988,
#12989,#12990,#12991,#12992,#12993,#12994,#12995,#12996,#12997,#12998,#12999,
#13000,#13001,#13002,#13003,#13004,#13005,#13006,#13007,#13008,#13009,#13010,
#13011,#13012,#13013,#13014,#13015,#13016,#13017,#13018,#13019,#13020,#13021,
#13022,#13023,#13024,#13025,#13026,#13027,#13028,#13029,#13030,#13031,#13032,
#13033,#13034,#13035,#13036,#13037,#13038,#13039),.UNSPECIFIED.,.F.,.F.,
(4,3,3,3,3,3,3,3,3,3,3,3,3,3,3,3,3,3,3,3,3,3,4),(-0.0308474254388288,-0.0282443142460501,
-0.0239308460091484,-0.0206152613794386,-0.0170461144143175,-0.0150701377107825,
-0.0131660090144569,-0.0115202578876498,-0.0103391767664952,-0.00917732807839727,
-0.00816993700961439,-0.0072574718319948,-0.00648885936575202,-0.00537659349968903,
-0.00470451931222791,-0.00408467784513401,-0.00323202309051337,-0.00269108370452265,
-0.00220561578410232,-0.00169529231285346,-0.00084764615642673,-0.000380223898580438,
0.),.UNSPECIFIED.);
#149=B_SPLINE_CURVE_WITH_KNOTS('',5,(#13197,#13198,#13199,#13200,#13201,
#13202,#13203,#13204,#13205,#13206,#13207,#13208,#13209,#13210,#13211,#13212,
#13213,#13214,#13215,#13216,#13217,#13218,#13219,#13220,#13221,#13222,#13223,
#13224,#13225,#13226,#13227,#13228,#13229,#13230,#13231,#13232,#13233,#13234,
#13235,#13236,#13237,#13238,#13239,#13240,#13241,#13242,#13243,#13244,#13245,
#13246,#13247,#13248,#13249,#13250,#13251,#13252,#13253,#13254,#13255,#13256,
#13257,#13258,#13259,#13260,#13261,#13262,#13263,#13264,#13265,#13266,#13267,
#13268,#13269,#13270),.UNSPECIFIED.,.F.,.F.,(6,1,1,1,1,1,1,1,1,1,1,1,1,
1,1,1,1,1,1,1,1,1,1,1,1,1,1,1,1,1,1,1,1,1,1,1,1,1,1,1,1,1,1,1,1,1,1,1,1,
1,1,1,1,1,1,1,1,1,1,1,1,1,1,1,1,1,1,1,1,6),(0.,0.0142857142857143,0.0285714285714286,
0.0428571428571429,0.0571428571428571,0.0714285714285714,0.0857142857142857,
0.1,0.114285714285714,0.128571428571429,0.142857142857143,0.157142857142857,
0.171428571428571,0.185714285714286,0.2,0.214285714285714,0.228571428571429,
0.242857142857143,0.257142857142857,0.271428571428571,0.285714285714286,
0.3,0.314285714285714,0.328571428571429,0.342857142857143,0.357142857142857,
0.371428571428571,0.385714285714286,0.4,0.414285714285714,0.428571428571429,
0.442857142857143,0.457142857142857,0.471428571428572,0.485714285714286,
0.5,0.514285714285714,0.528571428571429,0.542857142857143,0.557142857142857,
0.571428571428571,0.585714285714286,0.6,0.614285714285714,0.628571428571428,
0.642857142857142,0.657142857142857,0.671428571428571,0.685714285714285,
0.699999999999999,0.714285714285714,0.728571428571428,0.742857142857142,
0.757142857142856,0.771428571428571,0.785714285714285,0.799999999999999,
0.814285714285713,0.828571428571428,0.842857142857142,0.857142857142856,
0.87142857142857,0.885714285714284,0.899999999999999,0.914285714285713,
0.928571428571427,0.942857142857141,0.957142857142856,0.97142857142857,
1.),.UNSPECIFIED.);
#150=B_SPLINE_CURVE_WITH_KNOTS('',3,(#13271,#13272,#13273,#13274,#13275,
#13276,#13277,#13278,#13279,#13280,#13281,#13282,#13283,#13284,#13285,#13286,
#13287,#13288,#13289,#13290,#13291,#13292,#13293,#13294,#13295,#13296,#13297,
#13298,#13299,#13300,#13301,#13302,#13303,#13304,#13305,#13306,#13307,#13308,
#13309,#13310,#13311,#13312,#13313,#13314,#13315,#13316,#13317,#13318,#13319,
#13320,#13321,#13322,#13323,#13324,#13325,#13326,#13327,#13328,#13329,#13330,
#13331,#13332,#13333,#13334,#13335,#13336,#13337,#13338,#13339,#13340),
 .UNSPECIFIED.,.F.,.F.,(4,3,3,3,3,3,3,3,3,3,3,3,3,3,3,3,3,3,3,3,3,3,3,4),
(-0.41144900992668,-0.405504895550952,-0.398537948913654,-0.388735121571637,
-0.382214695372107,-0.37535087794608,-0.367728232965685,-0.356236725685507,
-0.347888396876633,-0.33768327976105,-0.326660059574477,-0.316483474477592,
-0.302658061103083,-0.289316835800213,-0.271192407406943,-0.255261428869757,
-0.231775298804757,-0.202135573441996,-0.161986280303818,-0.126192134093902,
-0.0754619856550688,-0.0360560111222661,-0.00196686536757399,0.),
 .UNSPECIFIED.);
#151=B_SPLINE_CURVE_WITH_KNOTS('',5,(#13492,#13493,#13494,#13495,#13496,
#13497,#13498,#13499,#13500,#13501,#13502,#13503,#13504,#13505,#13506,#13507,
#13508,#13509,#13510,#13511,#13512,#13513,#13514,#13515,#13516,#13517,#13518,
#13519,#13520,#13521,#13522,#13523,#13524,#13525,#13526,#13527,#13528,#13529,
#13530,#13531,#13532,#13533,#13534,#13535,#13536,#13537,#13538,#13539,#13540,
#13541,#13542,#13543,#13544,#13545,#13546,#13547,#13548,#13549,#13550,#13551,
#13552,#13553,#13554,#13555,#13556,#13557,#13558,#13559,#13560,#13561,#13562,
#13563,#13564,#13565),.UNSPECIFIED.,.F.,.F.,(6,1,1,1,1,1,1,1,1,1,1,1,1,
1,1,1,1,1,1,1,1,1,1,1,1,1,1,1,1,1,1,1,1,1,1,1,1,1,1,1,1,1,1,1,1,1,1,1,1,
1,1,1,1,1,1,1,1,1,1,1,1,1,1,1,1,1,1,1,1,6),(0.,0.0142857142857143,0.0285714285714286,
0.0428571428571429,0.0571428571428571,0.0714285714285714,0.0857142857142857,
0.1,0.114285714285714,0.128571428571429,0.142857142857143,0.157142857142857,
0.171428571428571,0.185714285714286,0.2,0.214285714285714,0.228571428571429,
0.242857142857143,0.257142857142857,0.271428571428571,0.285714285714286,
0.3,0.314285714285714,0.328571428571429,0.342857142857143,0.357142857142857,
0.371428571428571,0.385714285714286,0.4,0.414285714285714,0.428571428571429,
0.442857142857143,0.457142857142857,0.471428571428572,0.485714285714286,
0.5,0.514285714285714,0.528571428571429,0.542857142857143,0.557142857142857,
0.571428571428571,0.585714285714286,0.6,0.614285714285714,0.628571428571428,
0.642857142857142,0.657142857142857,0.671428571428571,0.685714285714285,
0.699999999999999,0.714285714285714,0.728571428571428,0.742857142857142,
0.757142857142856,0.771428571428571,0.785714285714285,0.799999999999999,
0.814285714285713,0.828571428571428,0.842857142857142,0.857142857142856,
0.87142857142857,0.885714285714284,0.899999999999999,0.914285714285713,
0.928571428571427,0.942857142857141,0.957142857142856,0.97142857142857,
1.),.UNSPECIFIED.);
#152=B_SPLINE_CURVE_WITH_KNOTS('',3,(#13567,#13568,#13569,#13570,#13571,
#13572,#13573,#13574,#13575,#13576,#13577,#13578,#13579,#13580,#13581,#13582,
#13583,#13584,#13585,#13586,#13587,#13588,#13589,#13590,#13591,#13592,#13593,
#13594,#13595,#13596,#13597,#13598,#13599,#13600,#13601,#13602,#13603,#13604,
#13605,#13606,#13607,#13608,#13609,#13610,#13611,#13612,#13613,#13614,#13615,
#13616,#13617,#13618,#13619,#13620,#13621,#13622,#13623,#13624,#13625,#13626,
#13627,#13628,#13629,#13630,#13631,#13632,#13633),.UNSPECIFIED.,.F.,.F.,
(4,3,3,3,3,3,3,3,3,3,3,3,3,3,3,3,3,3,3,3,3,3,4),(-0.0308474254052201,-0.0282443140946725,
-0.0239308458458541,-0.0206152612254046,-0.0170461143478486,-0.015070137591752,
-0.0131660090404763,-0.0115202579104168,-0.0103391767922971,-0.00917732808736861,
-0.0081699370073885,-0.00725747183607438,-0.00648885936953476,-0.00537659348374253,
-0.00470451929827472,-0.00408467783114113,-0.00323202309011053,-0.00269108370432218,
-0.00220561578425795,-0.00169529231400166,-0.000847646157000828,-0.000380223899135919,
0.),.UNSPECIFIED.);
#153=B_SPLINE_CURVE_WITH_KNOTS('',5,(#13791,#13792,#13793,#13794,#13795,
#13796,#13797,#13798,#13799,#13800,#13801,#13802,#13803,#13804,#13805,#13806,
#13807,#13808,#13809,#13810,#13811,#13812,#13813,#13814,#13815,#13816,#13817,
#13818,#13819,#13820,#13821,#13822,#13823,#13824,#13825,#13826,#13827,#13828,
#13829,#13830,#13831,#13832,#13833,#13834,#13835,#13836,#13837,#13838,#13839,
#13840,#13841,#13842,#13843,#13844,#13845,#13846,#13847,#13848,#13849,#13850,
#13851,#13852,#13853,#13854,#13855,#13856,#13857,#13858,#13859,#13860,#13861,
#13862,#13863,#13864),.UNSPECIFIED.,.F.,.F.,(6,1,1,1,1,1,1,1,1,1,1,1,1,
1,1,1,1,1,1,1,1,1,1,1,1,1,1,1,1,1,1,1,1,1,1,1,1,1,1,1,1,1,1,1,1,1,1,1,1,
1,1,1,1,1,1,1,1,1,1,1,1,1,1,1,1,1,1,1,1,6),(0.,0.0142857142857143,0.0285714285714286,
0.0428571428571429,0.0571428571428571,0.0714285714285714,0.0857142857142857,
0.1,0.114285714285714,0.128571428571429,0.142857142857143,0.157142857142857,
0.171428571428571,0.185714285714286,0.2,0.214285714285714,0.228571428571429,
0.242857142857143,0.257142857142857,0.271428571428571,0.285714285714286,
0.3,0.314285714285714,0.328571428571429,0.342857142857143,0.357142857142857,
0.371428571428571,0.385714285714286,0.4,0.414285714285714,0.428571428571429,
0.442857142857143,0.457142857142857,0.471428571428572,0.485714285714286,
0.5,0.514285714285714,0.528571428571429,0.542857142857143,0.557142857142857,
0.571428571428571,0.585714285714286,0.6,0.614285714285714,0.628571428571428,
0.642857142857142,0.657142857142857,0.671428571428571,0.685714285714285,
0.699999999999999,0.714285714285714,0.728571428571428,0.742857142857142,
0.757142857142856,0.771428571428571,0.785714285714285,0.799999999999999,
0.814285714285713,0.828571428571428,0.842857142857142,0.857142857142856,
0.87142857142857,0.885714285714284,0.899999999999999,0.914285714285713,
0.928571428571427,0.942857142857141,0.957142857142856,0.97142857142857,
1.),.UNSPECIFIED.);
#154=B_SPLINE_CURVE_WITH_KNOTS('',3,(#13865,#13866,#13867,#13868,#13869,
#13870,#13871,#13872,#13873,#13874,#13875,#13876,#13877,#13878,#13879,#13880,
#13881,#13882,#13883,#13884,#13885,#13886,#13887,#13888,#13889,#13890,#13891,
#13892,#13893,#13894,#13895,#13896,#13897,#13898,#13899,#13900,#13901,#13902,
#13903,#13904,#13905,#13906,#13907,#13908,#13909,#13910,#13911,#13912,#13913,
#13914,#13915,#13916,#13917,#13918,#13919,#13920,#13921,#13922,#13923,#13924,
#13925,#13926,#13927,#13928,#13929,#13930,#13931,#13932,#13933,#13934),
 .UNSPECIFIED.,.F.,.F.,(4,3,3,3,3,3,3,3,3,3,3,3,3,3,3,3,3,3,3,3,3,3,3,4),
(-0.411449009805915,-0.405504895443787,-0.398537948811133,-0.388735121455847,
-0.382214695257969,-0.375350877833497,-0.367728232855643,-0.356236725578904,
-0.347888396774101,-0.337683279662952,-0.326660059480431,-0.316483474386569,
-0.302658061019101,-0.289316835720957,-0.271192407372165,-0.25526142885209,
-0.231775298779651,-0.202135573443613,-0.161986280308302,-0.126192134070803,
-0.0754619857048084,-0.0360560114441301,-0.00196686623016366,0.),
 .UNSPECIFIED.);
#155=B_SPLINE_CURVE_WITH_KNOTS('',5,(#14086,#14087,#14088,#14089,#14090,
#14091,#14092,#14093,#14094,#14095,#14096,#14097,#14098,#14099,#14100,#14101,
#14102,#14103,#14104,#14105,#14106,#14107,#14108,#14109,#14110,#14111,#14112,
#14113,#14114,#14115,#14116,#14117,#14118,#14119,#14120,#14121,#14122,#14123,
#14124,#14125,#14126,#14127,#14128,#14129,#14130,#14131,#14132,#14133,#14134,
#14135,#14136,#14137,#14138,#14139,#14140,#14141,#14142,#14143,#14144,#14145,
#14146,#14147,#14148,#14149,#14150,#14151,#14152,#14153,#14154,#14155,#14156,
#14157,#14158,#14159),.UNSPECIFIED.,.F.,.F.,(6,1,1,1,1,1,1,1,1,1,1,1,1,
1,1,1,1,1,1,1,1,1,1,1,1,1,1,1,1,1,1,1,1,1,1,1,1,1,1,1,1,1,1,1,1,1,1,1,1,
1,1,1,1,1,1,1,1,1,1,1,1,1,1,1,1,1,1,1,1,6),(0.,0.0142857142857143,0.0285714285714286,
0.0428571428571429,0.0571428571428571,0.0714285714285714,0.0857142857142857,
0.1,0.114285714285714,0.128571428571429,0.142857142857143,0.157142857142857,
0.171428571428571,0.185714285714286,0.2,0.214285714285714,0.228571428571429,
0.242857142857143,0.257142857142857,0.271428571428571,0.285714285714286,
0.3,0.314285714285714,0.328571428571429,0.342857142857143,0.357142857142857,
0.371428571428571,0.385714285714286,0.4,0.414285714285714,0.428571428571429,
0.442857142857143,0.457142857142857,0.471428571428572,0.485714285714286,
0.5,0.514285714285714,0.528571428571429,0.542857142857143,0.557142857142857,
0.571428571428571,0.585714285714286,0.6,0.614285714285714,0.628571428571428,
0.642857142857142,0.657142857142857,0.671428571428571,0.685714285714285,
0.699999999999999,0.714285714285714,0.728571428571428,0.742857142857142,
0.757142857142856,0.771428571428571,0.785714285714285,0.799999999999999,
0.814285714285713,0.828571428571428,0.842857142857142,0.857142857142856,
0.87142857142857,0.885714285714284,0.899999999999999,0.914285714285713,
0.928571428571427,0.942857142857141,0.957142857142856,0.97142857142857,
1.),.UNSPECIFIED.);
#156=B_SPLINE_CURVE_WITH_KNOTS('',3,(#14161,#14162,#14163,#14164,#14165,
#14166,#14167,#14168,#14169,#14170,#14171,#14172,#14173,#14174,#14175,#14176,
#14177,#14178,#14179,#14180,#14181,#14182,#14183,#14184,#14185,#14186,#14187,
#14188,#14189,#14190,#14191,#14192,#14193,#14194,#14195,#14196,#14197,#14198,
#14199,#14200,#14201,#14202,#14203,#14204,#14205,#14206,#14207,#14208,#14209,
#14210,#14211,#14212,#14213,#14214,#14215,#14216,#14217,#14218,#14219,#14220,
#14221,#14222,#14223,#14224,#14225,#14226,#14227),.UNSPECIFIED.,.F.,.F.,
(4,3,3,3,3,3,3,3,3,3,3,3,3,3,3,3,3,3,3,3,3,3,4),(-0.0308474254313729,-0.0282443144331512,
-0.0239308462436385,-0.0206152616062002,-0.017046114491142,-0.0150701378789916,
-0.0131660089309141,-0.0115202578145499,-0.0103391766904584,-0.0091773280428693,
-0.00816993699591886,-0.00725747180427489,-0.00648885934148822,-0.00537659351838039,
-0.00470451932858284,-0.00408467786302119,-0.00323202308259216,-0.00269108369773592,
-0.00220561577775678,-0.00169529230541892,-0.00084764615270946,-0.000380223895080282,
0.),.UNSPECIFIED.);
#157=B_SPLINE_CURVE_WITH_KNOTS('',5,(#14385,#14386,#14387,#14388,#14389,
#14390,#14391,#14392,#14393,#14394,#14395,#14396,#14397,#14398,#14399,#14400,
#14401,#14402,#14403,#14404,#14405,#14406,#14407,#14408,#14409,#14410,#14411,
#14412,#14413,#14414,#14415,#14416,#14417,#14418,#14419,#14420,#14421,#14422,
#14423,#14424,#14425,#14426,#14427,#14428,#14429,#14430,#14431,#14432,#14433,
#14434,#14435,#14436,#14437,#14438,#14439,#14440,#14441,#14442,#14443,#14444,
#14445,#14446,#14447,#14448,#14449,#14450,#14451,#14452,#14453,#14454,#14455,
#14456,#14457,#14458),.UNSPECIFIED.,.F.,.F.,(6,1,1,1,1,1,1,1,1,1,1,1,1,
1,1,1,1,1,1,1,1,1,1,1,1,1,1,1,1,1,1,1,1,1,1,1,1,1,1,1,1,1,1,1,1,1,1,1,1,
1,1,1,1,1,1,1,1,1,1,1,1,1,1,1,1,1,1,1,1,6),(0.,0.0142857142857143,0.0285714285714286,
0.0428571428571429,0.0571428571428571,0.0714285714285714,0.0857142857142857,
0.1,0.114285714285714,0.128571428571429,0.142857142857143,0.157142857142857,
0.171428571428571,0.185714285714286,0.2,0.214285714285714,0.228571428571429,
0.242857142857143,0.257142857142857,0.271428571428571,0.285714285714286,
0.3,0.314285714285714,0.328571428571429,0.342857142857143,0.357142857142857,
0.371428571428571,0.385714285714286,0.4,0.414285714285714,0.428571428571429,
0.442857142857143,0.457142857142857,0.471428571428572,0.485714285714286,
0.5,0.514285714285714,0.528571428571429,0.542857142857143,0.557142857142857,
0.571428571428571,0.585714285714286,0.6,0.614285714285714,0.628571428571428,
0.642857142857142,0.657142857142857,0.671428571428571,0.685714285714285,
0.699999999999999,0.714285714285714,0.728571428571428,0.742857142857142,
0.757142857142856,0.771428571428571,0.785714285714285,0.799999999999999,
0.814285714285713,0.828571428571428,0.842857142857142,0.857142857142856,
0.87142857142857,0.885714285714284,0.899999999999999,0.914285714285713,
0.928571428571427,0.942857142857141,0.957142857142856,0.97142857142857,
1.),.UNSPECIFIED.);
#158=B_SPLINE_CURVE_WITH_KNOTS('',3,(#14459,#14460,#14461,#14462,#14463,
#14464,#14465,#14466,#14467,#14468,#14469,#14470,#14471,#14472,#14473,#14474,
#14475,#14476,#14477,#14478,#14479,#14480,#14481,#14482,#14483,#14484,#14485,
#14486,#14487,#14488,#14489,#14490,#14491,#14492,#14493,#14494,#14495,#14496,
#14497,#14498,#14499,#14500,#14501,#14502,#14503,#14504,#14505,#14506,#14507,
#14508,#14509,#14510,#14511,#14512,#14513,#14514,#14515,#14516,#14517,#14518,
#14519,#14520,#14521,#14522,#14523,#14524,#14525,#14526,#14527,#14528),
 .UNSPECIFIED.,.F.,.F.,(4,3,3,3,3,3,3,3,3,3,3,3,3,3,3,3,3,3,3,3,3,3,3,4),
(-0.411449009745582,-0.405504895379435,-0.398537948745384,-0.388735121403136,
-0.382214695205601,-0.375350877782795,-0.367728232806823,-0.35623672553161,
-0.347888396726707,-0.337683279620391,-0.326660059439279,-0.316483474349347,
-0.302658060997721,-0.289316835702375,-0.271192407460765,-0.255261428951979,
-0.231775298732412,-0.202135573328733,-0.161986280135987,-0.12619213402364,
-0.0754619855322879,-0.0360560073833462,-0.00196685495466459,0.),
 .UNSPECIFIED.);
#159=B_SPLINE_CURVE_WITH_KNOTS('',5,(#14680,#14681,#14682,#14683,#14684,
#14685,#14686,#14687,#14688,#14689,#14690,#14691,#14692,#14693,#14694,#14695,
#14696,#14697,#14698,#14699,#14700,#14701,#14702,#14703,#14704,#14705,#14706,
#14707,#14708,#14709,#14710,#14711,#14712,#14713,#14714,#14715,#14716,#14717,
#14718,#14719,#14720,#14721,#14722,#14723,#14724,#14725,#14726,#14727,#14728,
#14729,#14730,#14731,#14732,#14733,#14734,#14735,#14736,#14737,#14738,#14739,
#14740,#14741,#14742,#14743,#14744,#14745,#14746,#14747,#14748,#14749,#14750,
#14751,#14752,#14753),.UNSPECIFIED.,.F.,.F.,(6,1,1,1,1,1,1,1,1,1,1,1,1,
1,1,1,1,1,1,1,1,1,1,1,1,1,1,1,1,1,1,1,1,1,1,1,1,1,1,1,1,1,1,1,1,1,1,1,1,
1,1,1,1,1,1,1,1,1,1,1,1,1,1,1,1,1,1,1,1,6),(0.,0.0142857142857143,0.0285714285714286,
0.0428571428571429,0.0571428571428571,0.0714285714285714,0.0857142857142857,
0.1,0.114285714285714,0.128571428571429,0.142857142857143,0.157142857142857,
0.171428571428571,0.185714285714286,0.2,0.214285714285714,0.228571428571429,
0.242857142857143,0.257142857142857,0.271428571428571,0.285714285714286,
0.3,0.314285714285714,0.328571428571429,0.342857142857143,0.357142857142857,
0.371428571428571,0.385714285714286,0.4,0.414285714285714,0.428571428571429,
0.442857142857143,0.457142857142857,0.471428571428572,0.485714285714286,
0.5,0.514285714285714,0.528571428571429,0.542857142857143,0.557142857142857,
0.571428571428571,0.585714285714286,0.6,0.614285714285714,0.628571428571428,
0.642857142857142,0.657142857142857,0.671428571428571,0.685714285714285,
0.699999999999999,0.714285714285714,0.728571428571428,0.742857142857142,
0.757142857142856,0.771428571428571,0.785714285714285,0.799999999999999,
0.814285714285713,0.828571428571428,0.842857142857142,0.857142857142856,
0.87142857142857,0.885714285714284,0.899999999999999,0.914285714285713,
0.928571428571427,0.942857142857141,0.957142857142856,0.97142857142857,
1.),.UNSPECIFIED.);
#160=B_SPLINE_CURVE_WITH_KNOTS('',3,(#14755,#14756,#14757,#14758,#14759,
#14760,#14761,#14762,#14763,#14764,#14765,#14766,#14767,#14768,#14769,#14770,
#14771,#14772,#14773,#14774,#14775,#14776,#14777,#14778,#14779,#14780,#14781,
#14782,#14783,#14784,#14785,#14786,#14787,#14788,#14789,#14790,#14791,#14792,
#14793,#14794,#14795,#14796,#14797,#14798,#14799,#14800,#14801,#14802,#14803,
#14804,#14805,#14806,#14807,#14808,#14809,#14810,#14811,#14812,#14813,#14814,
#14815,#14816,#14817,#14818,#14819,#14820,#14821),.UNSPECIFIED.,.F.,.F.,
(4,3,3,3,3,3,3,3,3,3,3,3,3,3,3,3,3,3,3,3,3,3,4),(-0.0308474254096501,-0.028244313899376,
-0.0239308455956517,-0.020615260955671,-0.0170461143005811,-0.0150701375011353,
-0.0131660090769615,-0.0115202579423413,-0.0103391768283886,-0.00917732810453088,
-0.0081699370150875,-0.00725747185097503,-0.0064888593825484,-0.00537659347407927,
-0.00470451928981936,-0.00408467782188743,-0.00323202309462087,-0.00269108370824936,
-0.00220561578794048,-0.00169529231835461,-0.000847646159177307,-0.000380223901533956,
0.),.UNSPECIFIED.);
#161=B_SPLINE_CURVE_WITH_KNOTS('',5,(#14979,#14980,#14981,#14982,#14983,
#14984,#14985,#14986,#14987,#14988,#14989,#14990,#14991,#14992,#14993,#14994,
#14995,#14996,#14997,#14998,#14999,#15000,#15001,#15002,#15003,#15004,#15005,
#15006,#15007,#15008,#15009,#15010,#15011,#15012,#15013,#15014,#15015,#15016,
#15017,#15018,#15019,#15020,#15021,#15022,#15023,#15024,#15025,#15026,#15027,
#15028,#15029,#15030,#15031,#15032,#15033,#15034,#15035,#15036,#15037,#15038,
#15039,#15040,#15041,#15042,#15043,#15044,#15045,#15046,#15047,#15048,#15049,
#15050,#15051,#15052),.UNSPECIFIED.,.F.,.F.,(6,1,1,1,1,1,1,1,1,1,1,1,1,
1,1,1,1,1,1,1,1,1,1,1,1,1,1,1,1,1,1,1,1,1,1,1,1,1,1,1,1,1,1,1,1,1,1,1,1,
1,1,1,1,1,1,1,1,1,1,1,1,1,1,1,1,1,1,1,1,6),(0.,0.0142857142857143,0.0285714285714286,
0.0428571428571429,0.0571428571428571,0.0714285714285714,0.0857142857142857,
0.1,0.114285714285714,0.128571428571429,0.142857142857143,0.157142857142857,
0.171428571428571,0.185714285714286,0.2,0.214285714285714,0.228571428571429,
0.242857142857143,0.257142857142857,0.271428571428571,0.285714285714286,
0.3,0.314285714285714,0.328571428571429,0.342857142857143,0.357142857142857,
0.371428571428571,0.385714285714286,0.4,0.414285714285714,0.428571428571429,
0.442857142857143,0.457142857142857,0.471428571428572,0.485714285714286,
0.5,0.514285714285714,0.528571428571429,0.542857142857143,0.557142857142857,
0.571428571428571,0.585714285714286,0.6,0.614285714285714,0.628571428571428,
0.642857142857142,0.657142857142857,0.671428571428571,0.685714285714285,
0.699999999999999,0.714285714285714,0.728571428571428,0.742857142857142,
0.757142857142856,0.771428571428571,0.785714285714285,0.799999999999999,
0.814285714285713,0.828571428571428,0.842857142857142,0.857142857142856,
0.87142857142857,0.885714285714284,0.899999999999999,0.914285714285713,
0.928571428571427,0.942857142857141,0.957142857142856,0.97142857142857,
1.),.UNSPECIFIED.);
#162=B_SPLINE_CURVE_WITH_KNOTS('',3,(#15053,#15054,#15055,#15056,#15057,
#15058,#15059,#15060,#15061,#15062,#15063,#15064,#15065,#15066,#15067,#15068,
#15069,#15070,#15071,#15072,#15073,#15074,#15075,#15076,#15077,#15078,#15079,
#15080,#15081,#15082,#15083,#15084,#15085,#15086,#15087,#15088,#15089,#15090,
#15091,#15092,#15093,#15094,#15095,#15096,#15097,#15098,#15099,#15100,#15101,
#15102,#15103,#15104,#15105,#15106,#15107,#15108,#15109,#15110,#15111,#15112,
#15113,#15114,#15115,#15116,#15117,#15118,#15119,#15120,#15121,#15122),
 .UNSPECIFIED.,.F.,.F.,(4,3,3,3,3,3,3,3,3,3,3,3,3,3,3,3,3,3,3,3,3,3,3,4),
(-0.411449009865562,-0.4055048954869,-0.398537948850747,-0.388735121518256,
-0.382214695319647,-0.375350877895016,-0.3677282329171,-0.35623672563844,
-0.347888396831227,-0.337683279715536,-0.326660059528631,-0.316483474438613,
-0.302658061094389,-0.28931683580642,-0.271192407552387,-0.255261429122638,
-0.231775298922887,-0.202135573548005,-0.161986280573123,-0.126192134261937,
-0.0754619859222758,-0.0360560139042322,-0.00196687400591684,0.),
 .UNSPECIFIED.);
#163=B_SPLINE_CURVE_WITH_KNOTS('',5,(#15274,#15275,#15276,#15277,#15278,
#15279,#15280,#15281,#15282,#15283,#15284,#15285,#15286,#15287,#15288,#15289,
#15290,#15291,#15292,#15293,#15294,#15295,#15296,#15297,#15298,#15299,#15300,
#15301,#15302,#15303,#15304,#15305,#15306,#15307,#15308,#15309,#15310,#15311,
#15312,#15313,#15314,#15315,#15316,#15317,#15318,#15319,#15320,#15321,#15322,
#15323,#15324,#15325,#15326,#15327,#15328,#15329,#15330,#15331,#15332,#15333,
#15334,#15335,#15336,#15337,#15338,#15339,#15340,#15341,#15342,#15343,#15344,
#15345,#15346,#15347),.UNSPECIFIED.,.F.,.F.,(6,1,1,1,1,1,1,1,1,1,1,1,1,
1,1,1,1,1,1,1,1,1,1,1,1,1,1,1,1,1,1,1,1,1,1,1,1,1,1,1,1,1,1,1,1,1,1,1,1,
1,1,1,1,1,1,1,1,1,1,1,1,1,1,1,1,1,1,1,1,6),(0.,0.0142857142857143,0.0285714285714286,
0.0428571428571429,0.0571428571428571,0.0714285714285714,0.0857142857142857,
0.1,0.114285714285714,0.128571428571429,0.142857142857143,0.157142857142857,
0.171428571428571,0.185714285714286,0.2,0.214285714285714,0.228571428571429,
0.242857142857143,0.257142857142857,0.271428571428571,0.285714285714286,
0.3,0.314285714285714,0.328571428571429,0.342857142857143,0.357142857142857,
0.371428571428571,0.385714285714286,0.4,0.414285714285714,0.428571428571429,
0.442857142857143,0.457142857142857,0.471428571428572,0.485714285714286,
0.5,0.514285714285714,0.528571428571429,0.542857142857143,0.557142857142857,
0.571428571428571,0.585714285714286,0.6,0.614285714285714,0.628571428571428,
0.642857142857142,0.657142857142857,0.671428571428571,0.685714285714285,
0.699999999999999,0.714285714285714,0.728571428571428,0.742857142857142,
0.757142857142856,0.771428571428571,0.785714285714285,0.799999999999999,
0.814285714285713,0.828571428571428,0.842857142857142,0.857142857142856,
0.87142857142857,0.885714285714284,0.899999999999999,0.914285714285713,
0.928571428571427,0.942857142857141,0.957142857142856,0.97142857142857,
1.),.UNSPECIFIED.);
#164=B_SPLINE_CURVE_WITH_KNOTS('',3,(#15349,#15350,#15351,#15352,#15353,
#15354,#15355,#15356,#15357,#15358,#15359,#15360,#15361,#15362,#15363,#15364,
#15365,#15366,#15367,#15368,#15369,#15370,#15371,#15372,#15373,#15374,#15375,
#15376,#15377,#15378,#15379,#15380,#15381,#15382,#15383,#15384,#15385,#15386,
#15387,#15388,#15389,#15390,#15391,#15392,#15393,#15394,#15395,#15396,#15397,
#15398,#15399,#15400,#15401,#15402,#15403,#15404,#15405,#15406,#15407,#15408,
#15409,#15410,#15411,#15412,#15413,#15414,#15415),.UNSPECIFIED.,.F.,.F.,
(4,3,3,3,3,3,3,3,3,3,3,3,3,3,3,3,3,3,3,3,3,3,4),(-0.0308474254361046,-0.0282443142716837,
-0.0239308460693387,-0.0206152614403016,-0.0170461144189006,-0.0150701377175538,
-0.0131660090058279,-0.0115202578800994,-0.0103391767587464,-0.00917732807603053,
-0.0081699370085221,-0.00725747183125426,-0.00648885936500699,-0.00537659349888438,
-0.00470451931152384,-0.00408467784453854,-0.00323202309003581,-0.00269108370418276,
-0.00220561578378896,-0.00169529231258491,-0.000847646156292456,-0.00038022389874333,
0.),.UNSPECIFIED.);
#165=B_SPLINE_CURVE_WITH_KNOTS('',5,(#15573,#15574,#15575,#15576,#15577,
#15578,#15579,#15580,#15581,#15582,#15583,#15584,#15585,#15586,#15587,#15588,
#15589,#15590,#15591,#15592,#15593,#15594,#15595,#15596,#15597,#15598,#15599,
#15600,#15601,#15602,#15603,#15604,#15605,#15606,#15607,#15608,#15609,#15610,
#15611,#15612,#15613,#15614,#15615,#15616,#15617,#15618,#15619,#15620,#15621,
#15622,#15623,#15624,#15625,#15626,#15627,#15628,#15629,#15630,#15631,#15632,
#15633,#15634,#15635,#15636,#15637,#15638,#15639,#15640,#15641,#15642,#15643,
#15644,#15645,#15646),.UNSPECIFIED.,.F.,.F.,(6,1,1,1,1,1,1,1,1,1,1,1,1,
1,1,1,1,1,1,1,1,1,1,1,1,1,1,1,1,1,1,1,1,1,1,1,1,1,1,1,1,1,1,1,1,1,1,1,1,
1,1,1,1,1,1,1,1,1,1,1,1,1,1,1,1,1,1,1,1,6),(0.,0.0142857142857143,0.0285714285714286,
0.0428571428571429,0.0571428571428571,0.0714285714285714,0.0857142857142857,
0.1,0.114285714285714,0.128571428571429,0.142857142857143,0.157142857142857,
0.171428571428571,0.185714285714286,0.2,0.214285714285714,0.228571428571429,
0.242857142857143,0.257142857142857,0.271428571428571,0.285714285714286,
0.3,0.314285714285714,0.328571428571429,0.342857142857143,0.357142857142857,
0.371428571428571,0.385714285714286,0.4,0.414285714285714,0.428571428571429,
0.442857142857143,0.457142857142857,0.471428571428572,0.485714285714286,
0.5,0.514285714285714,0.528571428571429,0.542857142857143,0.557142857142857,
0.571428571428571,0.585714285714286,0.6,0.614285714285714,0.628571428571428,
0.642857142857142,0.657142857142857,0.671428571428571,0.685714285714285,
0.699999999999999,0.714285714285714,0.728571428571428,0.742857142857142,
0.757142857142856,0.771428571428571,0.785714285714285,0.799999999999999,
0.814285714285713,0.828571428571428,0.842857142857142,0.857142857142856,
0.87142857142857,0.885714285714284,0.899999999999999,0.914285714285713,
0.928571428571427,0.942857142857141,0.957142857142856,0.97142857142857,
1.),.UNSPECIFIED.);
#166=B_SPLINE_CURVE_WITH_KNOTS('',3,(#15647,#15648,#15649,#15650,#15651,
#15652,#15653,#15654,#15655,#15656,#15657,#15658,#15659,#15660,#15661,#15662,
#15663,#15664,#15665,#15666,#15667,#15668,#15669,#15670,#15671,#15672,#15673,
#15674,#15675,#15676,#15677,#15678,#15679,#15680,#15681,#15682,#15683,#15684,
#15685,#15686,#15687,#15688,#15689,#15690,#15691,#15692,#15693,#15694,#15695,
#15696,#15697,#15698,#15699,#15700,#15701,#15702,#15703,#15704,#15705,#15706,
#15707,#15708,#15709,#15710,#15711,#15712,#15713,#15714,#15715,#15716),
 .UNSPECIFIED.,.F.,.F.,(4,3,3,3,3,3,3,3,3,3,3,3,3,3,3,3,3,3,3,3,3,3,3,4),
(-0.411449009993053,-0.405504895610899,-0.398537948972071,-0.388735121637185,
-0.382214695436393,-0.37535087801037,-0.36772823302889,-0.356236725746737,
-0.347888396936899,-0.337683279821287,-0.326660059631445,-0.316483474534432,
-0.3026580611645,-0.28931683586772,-0.271192407496477,-0.255261428976351,
-0.231775298863032,-0.202135573489481,-0.161986280301393,-0.126192134011822,
-0.0754619855028801,-0.0360560096614338,-0.00196686194487841,0.),
 .UNSPECIFIED.);
#167=B_SPLINE_CURVE_WITH_KNOTS('',5,(#15868,#15869,#15870,#15871,#15872,
#15873,#15874,#15875,#15876,#15877,#15878,#15879,#15880,#15881,#15882,#15883,
#15884,#15885,#15886,#15887,#15888,#15889,#15890,#15891,#15892,#15893,#15894,
#15895,#15896,#15897,#15898,#15899,#15900,#15901,#15902,#15903,#15904,#15905,
#15906,#15907,#15908,#15909,#15910,#15911,#15912,#15913,#15914,#15915,#15916,
#15917,#15918,#15919,#15920,#15921,#15922,#15923,#15924,#15925,#15926,#15927,
#15928,#15929,#15930,#15931,#15932,#15933,#15934,#15935,#15936,#15937,#15938,
#15939,#15940,#15941),.UNSPECIFIED.,.F.,.F.,(6,1,1,1,1,1,1,1,1,1,1,1,1,
1,1,1,1,1,1,1,1,1,1,1,1,1,1,1,1,1,1,1,1,1,1,1,1,1,1,1,1,1,1,1,1,1,1,1,1,
1,1,1,1,1,1,1,1,1,1,1,1,1,1,1,1,1,1,1,1,6),(0.,0.0142857142857143,0.0285714285714286,
0.0428571428571429,0.0571428571428571,0.0714285714285714,0.0857142857142857,
0.1,0.114285714285714,0.128571428571429,0.142857142857143,0.157142857142857,
0.171428571428571,0.185714285714286,0.2,0.214285714285714,0.228571428571429,
0.242857142857143,0.257142857142857,0.271428571428571,0.285714285714286,
0.3,0.314285714285714,0.328571428571429,0.342857142857143,0.357142857142857,
0.371428571428571,0.385714285714286,0.4,0.414285714285714,0.428571428571429,
0.442857142857143,0.457142857142857,0.471428571428572,0.485714285714286,
0.5,0.514285714285714,0.528571428571429,0.542857142857143,0.557142857142857,
0.571428571428571,0.585714285714286,0.6,0.614285714285714,0.628571428571428,
0.642857142857142,0.657142857142857,0.671428571428571,0.685714285714285,
0.699999999999999,0.714285714285714,0.728571428571428,0.742857142857142,
0.757142857142856,0.771428571428571,0.785714285714285,0.799999999999999,
0.814285714285713,0.828571428571428,0.842857142857142,0.857142857142856,
0.87142857142857,0.885714285714284,0.899999999999999,0.914285714285713,
0.928571428571427,0.942857142857141,0.957142857142856,0.97142857142857,
1.),.UNSPECIFIED.);
#168=B_SPLINE_CURVE_WITH_KNOTS('',3,(#15943,#15944,#15945,#15946,#15947,
#15948,#15949,#15950,#15951,#15952,#15953,#15954,#15955,#15956,#15957,#15958,
#15959,#15960,#15961,#15962,#15963,#15964,#15965,#15966,#15967,#15968,#15969,
#15970,#15971,#15972,#15973,#15974,#15975,#15976,#15977,#15978,#15979,#15980,
#15981,#15982,#15983,#15984,#15985,#15986,#15987,#15988,#15989,#15990,#15991,
#15992,#15993,#15994,#15995,#15996,#15997,#15998,#15999,#16000,#16001,#16002,
#16003,#16004,#16005,#16006,#16007,#16008,#16009),.UNSPECIFIED.,.F.,.F.,
(4,3,3,3,3,3,3,3,3,3,3,3,3,3,3,3,3,3,3,3,3,3,4),(-0.0308474254372875,-0.0282443142425791,
-0.0239308460054441,-0.0206152613763472,-0.0170461144127407,-0.0150701377079118,
-0.0131660090146465,-0.0115202578878157,-0.0103391767667528,-0.00917732807920022,
-0.00816993700966646,-0.00725747183268602,-0.00648885936638244,-0.00537659349841556,
-0.00470451931111362,-0.00408467784397183,-0.00323202309066985,-0.00269108370466403,
-0.00220561578425269,-0.00169529231308492,-0.00084764615654246,-0.000380223898520597,
0.),.UNSPECIFIED.);
#169=B_SPLINE_CURVE_WITH_KNOTS('',5,(#16167,#16168,#16169,#16170,#16171,
#16172,#16173,#16174,#16175,#16176,#16177,#16178,#16179,#16180,#16181,#16182,
#16183,#16184,#16185,#16186,#16187,#16188,#16189,#16190,#16191,#16192,#16193,
#16194,#16195,#16196,#16197,#16198,#16199,#16200,#16201,#16202,#16203,#16204,
#16205,#16206,#16207,#16208,#16209,#16210,#16211,#16212,#16213,#16214,#16215,
#16216,#16217,#16218,#16219,#16220,#16221,#16222,#16223,#16224,#16225,#16226,
#16227,#16228,#16229,#16230,#16231,#16232,#16233,#16234,#16235,#16236,#16237,
#16238,#16239,#16240),.UNSPECIFIED.,.F.,.F.,(6,1,1,1,1,1,1,1,1,1,1,1,1,
1,1,1,1,1,1,1,1,1,1,1,1,1,1,1,1,1,1,1,1,1,1,1,1,1,1,1,1,1,1,1,1,1,1,1,1,
1,1,1,1,1,1,1,1,1,1,1,1,1,1,1,1,1,1,1,1,6),(0.,0.0142857142857143,0.0285714285714286,
0.0428571428571429,0.0571428571428571,0.0714285714285714,0.0857142857142857,
0.1,0.114285714285714,0.128571428571429,0.142857142857143,0.157142857142857,
0.171428571428571,0.185714285714286,0.2,0.214285714285714,0.228571428571429,
0.242857142857143,0.257142857142857,0.271428571428571,0.285714285714286,
0.3,0.314285714285714,0.328571428571429,0.342857142857143,0.357142857142857,
0.371428571428571,0.385714285714286,0.4,0.414285714285714,0.428571428571429,
0.442857142857143,0.457142857142857,0.471428571428572,0.485714285714286,
0.5,0.514285714285714,0.528571428571429,0.542857142857143,0.557142857142857,
0.571428571428571,0.585714285714286,0.6,0.614285714285714,0.628571428571428,
0.642857142857142,0.657142857142857,0.671428571428571,0.685714285714285,
0.699999999999999,0.714285714285714,0.728571428571428,0.742857142857142,
0.757142857142856,0.771428571428571,0.785714285714285,0.799999999999999,
0.814285714285713,0.828571428571428,0.842857142857142,0.857142857142856,
0.87142857142857,0.885714285714284,0.899999999999999,0.914285714285713,
0.928571428571427,0.942857142857141,0.957142857142856,0.97142857142857,
1.),.UNSPECIFIED.);
#170=B_SPLINE_CURVE_WITH_KNOTS('',3,(#16241,#16242,#16243,#16244,#16245,
#16246,#16247,#16248,#16249,#16250,#16251,#16252,#16253,#16254,#16255,#16256,
#16257,#16258,#16259,#16260,#16261,#16262,#16263,#16264,#16265,#16266,#16267,
#16268,#16269,#16270,#16271,#16272,#16273,#16274,#16275,#16276,#16277,#16278,
#16279,#16280,#16281,#16282,#16283,#16284,#16285,#16286,#16287,#16288,#16289,
#16290,#16291,#16292,#16293,#16294,#16295,#16296,#16297,#16298,#16299,#16300,
#16301,#16302,#16303,#16304,#16305,#16306,#16307,#16308,#16309,#16310),
 .UNSPECIFIED.,.F.,.F.,(4,3,3,3,3,3,3,3,3,3,3,3,3,3,3,3,3,3,3,3,3,3,3,4),
(-0.411449009936769,-0.405504895560803,-0.398537948923531,-0.388735121582206,
-0.382214695382425,-0.375350877956282,-0.36772823297609,-0.356236725695587,
-0.347888396886988,-0.337683279771699,-0.326660059584262,-0.316483474487346,
-0.302658061115119,-0.289316835813513,-0.271192407420841,-0.2552614288874,
-0.231775298819437,-0.20213557344945,-0.161986280299213,-0.126192134097661,
-0.075461985664044,-0.0360560111596636,-0.00196686546694207,0.),
 .UNSPECIFIED.);
#171=B_SPLINE_CURVE_WITH_KNOTS('',5,(#16462,#16463,#16464,#16465,#16466,
#16467,#16468,#16469,#16470,#16471,#16472,#16473,#16474,#16475,#16476,#16477,
#16478,#16479,#16480,#16481,#16482,#16483,#16484,#16485,#16486,#16487,#16488,
#16489,#16490,#16491,#16492,#16493,#16494,#16495,#16496,#16497,#16498,#16499,
#16500,#16501,#16502,#16503,#16504,#16505,#16506,#16507,#16508,#16509,#16510,
#16511,#16512,#16513,#16514,#16515,#16516,#16517,#16518,#16519,#16520,#16521,
#16522,#16523,#16524,#16525,#16526,#16527,#16528,#16529,#16530,#16531,#16532,
#16533,#16534,#16535),.UNSPECIFIED.,.F.,.F.,(6,1,1,1,1,1,1,1,1,1,1,1,1,
1,1,1,1,1,1,1,1,1,1,1,1,1,1,1,1,1,1,1,1,1,1,1,1,1,1,1,1,1,1,1,1,1,1,1,1,
1,1,1,1,1,1,1,1,1,1,1,1,1,1,1,1,1,1,1,1,6),(0.,0.0142857142857143,0.0285714285714286,
0.0428571428571429,0.0571428571428571,0.0714285714285714,0.0857142857142857,
0.1,0.114285714285714,0.128571428571429,0.142857142857143,0.157142857142857,
0.171428571428571,0.185714285714286,0.2,0.214285714285714,0.228571428571429,
0.242857142857143,0.257142857142857,0.271428571428571,0.285714285714286,
0.3,0.314285714285714,0.328571428571429,0.342857142857143,0.357142857142857,
0.371428571428571,0.385714285714286,0.4,0.414285714285714,0.428571428571429,
0.442857142857143,0.457142857142857,0.471428571428572,0.485714285714286,
0.5,0.514285714285714,0.528571428571429,0.542857142857143,0.557142857142857,
0.571428571428571,0.585714285714286,0.6,0.614285714285714,0.628571428571428,
0.642857142857142,0.657142857142857,0.671428571428571,0.685714285714285,
0.699999999999999,0.714285714285714,0.728571428571428,0.742857142857142,
0.757142857142856,0.771428571428571,0.785714285714285,0.799999999999999,
0.814285714285713,0.828571428571428,0.842857142857142,0.857142857142856,
0.87142857142857,0.885714285714284,0.899999999999999,0.914285714285713,
0.928571428571427,0.942857142857141,0.957142857142856,0.97142857142857,
1.),.UNSPECIFIED.);
#172=B_SPLINE_CURVE_WITH_KNOTS('',3,(#16537,#16538,#16539,#16540,#16541,
#16542,#16543,#16544,#16545,#16546,#16547,#16548,#16549,#16550,#16551,#16552,
#16553,#16554,#16555,#16556,#16557,#16558,#16559,#16560,#16561,#16562,#16563,
#16564,#16565,#16566,#16567,#16568,#16569,#16570,#16571,#16572,#16573,#16574,
#16575,#16576,#16577,#16578,#16579,#16580,#16581,#16582,#16583,#16584,#16585,
#16586,#16587,#16588,#16589,#16590,#16591,#16592,#16593,#16594,#16595,#16596,
#16597,#16598,#16599,#16600,#16601,#16602,#16603),.UNSPECIFIED.,.F.,.F.,
(4,3,3,3,3,3,3,3,3,3,3,3,3,3,3,3,3,3,3,3,3,3,4),(-0.0308474254273919,-0.0282443140912033,
-0.023930845835951,-0.0206152612175604,-0.017046114348032,-0.0150701375777768,
-0.0131660090603802,-0.0115202579278327,-0.0103391768090652,-0.00917732809722278,
-0.00816993701457461,-0.00725747184403407,-0.00648885937658713,-0.00537659348549602,
-0.00470451929980902,-0.00408467783206431,-0.00323202309310146,-0.0026910837068358,
-0.00220561578639057,-0.00169529231588426,-0.00084764615794213,-0.000380223899718856,
0.),.UNSPECIFIED.);
#173=B_SPLINE_CURVE_WITH_KNOTS('',5,(#16761,#16762,#16763,#16764,#16765,
#16766,#16767,#16768,#16769,#16770,#16771,#16772,#16773,#16774,#16775,#16776,
#16777,#16778,#16779,#16780,#16781,#16782,#16783,#16784,#16785,#16786,#16787,
#16788,#16789,#16790,#16791,#16792,#16793,#16794,#16795,#16796,#16797,#16798,
#16799,#16800,#16801,#16802,#16803,#16804,#16805,#16806,#16807,#16808,#16809,
#16810,#16811,#16812,#16813,#16814,#16815,#16816,#16817,#16818,#16819,#16820,
#16821,#16822,#16823,#16824,#16825,#16826,#16827,#16828,#16829,#16830,#16831,
#16832,#16833,#16834),.UNSPECIFIED.,.F.,.F.,(6,1,1,1,1,1,1,1,1,1,1,1,1,
1,1,1,1,1,1,1,1,1,1,1,1,1,1,1,1,1,1,1,1,1,1,1,1,1,1,1,1,1,1,1,1,1,1,1,1,
1,1,1,1,1,1,1,1,1,1,1,1,1,1,1,1,1,1,1,1,6),(0.,0.0142857142857143,0.0285714285714286,
0.0428571428571429,0.0571428571428571,0.0714285714285714,0.0857142857142857,
0.1,0.114285714285714,0.128571428571429,0.142857142857143,0.157142857142857,
0.171428571428571,0.185714285714286,0.2,0.214285714285714,0.228571428571429,
0.242857142857143,0.257142857142857,0.271428571428571,0.285714285714286,
0.3,0.314285714285714,0.328571428571429,0.342857142857143,0.357142857142857,
0.371428571428571,0.385714285714286,0.4,0.414285714285714,0.428571428571429,
0.442857142857143,0.457142857142857,0.471428571428572,0.485714285714286,
0.5,0.514285714285714,0.528571428571429,0.542857142857143,0.557142857142857,
0.571428571428571,0.585714285714286,0.6,0.614285714285714,0.628571428571428,
0.642857142857142,0.657142857142857,0.671428571428571,0.685714285714285,
0.699999999999999,0.714285714285714,0.728571428571428,0.742857142857142,
0.757142857142856,0.771428571428571,0.785714285714285,0.799999999999999,
0.814285714285713,0.828571428571428,0.842857142857142,0.857142857142856,
0.87142857142857,0.885714285714284,0.899999999999999,0.914285714285713,
0.928571428571427,0.942857142857141,0.957142857142856,0.97142857142857,
1.),.UNSPECIFIED.);
#174=B_SPLINE_CURVE_WITH_KNOTS('',3,(#16835,#16836,#16837,#16838,#16839,
#16840,#16841,#16842,#16843,#16844,#16845,#16846,#16847,#16848,#16849,#16850,
#16851,#16852,#16853,#16854,#16855,#16856,#16857,#16858,#16859,#16860,#16861,
#16862,#16863,#16864,#16865,#16866,#16867,#16868,#16869,#16870,#16871,#16872,
#16873,#16874,#16875,#16876,#16877,#16878,#16879,#16880,#16881,#16882,#16883,
#16884,#16885,#16886,#16887,#16888,#16889,#16890,#16891,#16892,#16893,#16894,
#16895,#16896,#16897,#16898,#16899,#16900,#16901,#16902,#16903,#16904),
 .UNSPECIFIED.,.F.,.F.,(4,3,3,3,3,3,3,3,3,3,3,3,3,3,3,3,3,3,3,3,3,3,3,4),
(-0.411449009732374,-0.405504895374025,-0.398537948743379,-0.388735121385456,
-0.382214695188797,-0.375350877765784,-0.367728232789201,-0.356236725514539,
-0.347888396711252,-0.337683279600152,-0.326660059420458,-0.316483474327811,
-0.302658060968815,-0.289316835675101,-0.271192407321049,-0.25526142880334,
-0.231775298738104,-0.202135573394745,-0.161986280278011,-0.12619213408638,
-0.075461986045109,-0.0360560119938936,-0.00196686781714211,0.),
 .UNSPECIFIED.);
#175=B_SPLINE_CURVE_WITH_KNOTS('',5,(#17056,#17057,#17058,#17059,#17060,
#17061,#17062,#17063,#17064,#17065,#17066,#17067,#17068,#17069,#17070,#17071,
#17072,#17073,#17074,#17075,#17076,#17077,#17078,#17079,#17080,#17081,#17082,
#17083,#17084,#17085,#17086,#17087,#17088,#17089,#17090,#17091,#17092,#17093,
#17094,#17095,#17096,#17097,#17098,#17099,#17100,#17101,#17102,#17103,#17104,
#17105,#17106,#17107,#17108,#17109,#17110,#17111,#17112,#17113,#17114,#17115,
#17116,#17117,#17118,#17119,#17120,#17121,#17122,#17123,#17124,#17125,#17126,
#17127,#17128,#17129),.UNSPECIFIED.,.F.,.F.,(6,1,1,1,1,1,1,1,1,1,1,1,1,
1,1,1,1,1,1,1,1,1,1,1,1,1,1,1,1,1,1,1,1,1,1,1,1,1,1,1,1,1,1,1,1,1,1,1,1,
1,1,1,1,1,1,1,1,1,1,1,1,1,1,1,1,1,1,1,1,6),(0.,0.0142857142857143,0.0285714285714286,
0.0428571428571429,0.0571428571428571,0.0714285714285714,0.0857142857142857,
0.1,0.114285714285714,0.128571428571429,0.142857142857143,0.157142857142857,
0.171428571428571,0.185714285714286,0.2,0.214285714285714,0.228571428571429,
0.242857142857143,0.257142857142857,0.271428571428571,0.285714285714286,
0.3,0.314285714285714,0.328571428571429,0.342857142857143,0.357142857142857,
0.371428571428571,0.385714285714286,0.4,0.414285714285714,0.428571428571429,
0.442857142857143,0.457142857142857,0.471428571428572,0.485714285714286,
0.5,0.514285714285714,0.528571428571429,0.542857142857143,0.557142857142857,
0.571428571428571,0.585714285714286,0.6,0.614285714285714,0.628571428571428,
0.642857142857142,0.657142857142857,0.671428571428571,0.685714285714285,
0.699999999999999,0.714285714285714,0.728571428571428,0.742857142857142,
0.757142857142856,0.771428571428571,0.785714285714285,0.799999999999999,
0.814285714285713,0.828571428571428,0.842857142857142,0.857142857142856,
0.87142857142857,0.885714285714284,0.899999999999999,0.914285714285713,
0.928571428571427,0.942857142857141,0.957142857142856,0.97142857142857,
1.),.UNSPECIFIED.);
#176=B_SPLINE_CURVE_WITH_KNOTS('',3,(#17131,#17132,#17133,#17134,#17135,
#17136,#17137,#17138,#17139,#17140,#17141,#17142,#17143,#17144,#17145,#17146,
#17147,#17148,#17149,#17150,#17151,#17152,#17153,#17154,#17155,#17156,#17157,
#17158,#17159,#17160,#17161,#17162,#17163,#17164,#17165,#17166,#17167,#17168,
#17169,#17170,#17171,#17172,#17173,#17174,#17175,#17176,#17177,#17178,#17179,
#17180,#17181,#17182,#17183,#17184,#17185,#17186,#17187,#17188,#17189,#17190,
#17191,#17192,#17193,#17194,#17195,#17196,#17197,#17198,#17199,#17200,#17201,
#17202,#17203,#17204,#17205,#17206,#17207,#17208,#17209,#17210,#17211,#17212),
 .UNSPECIFIED.,.F.,.F.,(4,3,3,3,3,3,3,3,3,3,3,3,3,3,3,3,3,3,3,3,3,3,3,3,
3,3,3,4),(-0.0308474254798612,-0.029574376059012,-0.0279034614454273,-0.0261594951050881,
-0.0245245266610201,-0.0244638420994598,-0.0235024106936745,-0.0226524167819541,
-0.0218081022887322,-0.0210633233132742,-0.0203818283699597,-0.0196859172472405,
-0.0190140811746369,-0.0183610672845718,-0.0175680780754909,-0.0168470831907521,
-0.0157941404913301,-0.0150253842943035,-0.0145558410351065,-0.0144056441754732,
-0.0143445590752705,-0.0129617214128992,-0.0112953999186002,-0.00949202192895945,
-0.00761828414789307,-0.00419987046129966,-0.00201831189392491,0.),
 .UNSPECIFIED.);
#177=B_SPLINE_CURVE_WITH_KNOTS('',5,(#17370,#17371,#17372,#17373,#17374,
#17375,#17376,#17377,#17378,#17379,#17380,#17381,#17382,#17383,#17384,#17385,
#17386,#17387,#17388,#17389,#17390,#17391,#17392,#17393,#17394,#17395,#17396,
#17397,#17398,#17399,#17400,#17401,#17402,#17403,#17404,#17405,#17406,#17407,
#17408,#17409,#17410,#17411,#17412,#17413,#17414,#17415,#17416,#17417,#17418,
#17419,#17420,#17421,#17422,#17423,#17424,#17425,#17426,#17427,#17428,#17429,
#17430,#17431,#17432,#17433,#17434,#17435,#17436,#17437,#17438,#17439,#17440,
#17441,#17442,#17443),.UNSPECIFIED.,.F.,.F.,(6,1,1,1,1,1,1,1,1,1,1,1,1,
1,1,1,1,1,1,1,1,1,1,1,1,1,1,1,1,1,1,1,1,1,1,1,1,1,1,1,1,1,1,1,1,1,1,1,1,
1,1,1,1,1,1,1,1,1,1,1,1,1,1,1,1,1,1,1,1,6),(0.,0.0142857142857143,0.0285714285714286,
0.0428571428571429,0.0571428571428571,0.0714285714285714,0.0857142857142857,
0.1,0.114285714285714,0.128571428571429,0.142857142857143,0.157142857142857,
0.171428571428571,0.185714285714286,0.2,0.214285714285714,0.228571428571429,
0.242857142857143,0.257142857142857,0.271428571428571,0.285714285714286,
0.3,0.314285714285714,0.328571428571429,0.342857142857143,0.357142857142857,
0.371428571428571,0.385714285714286,0.4,0.414285714285714,0.428571428571429,
0.442857142857143,0.457142857142857,0.471428571428572,0.485714285714286,
0.5,0.514285714285714,0.528571428571429,0.542857142857143,0.557142857142857,
0.571428571428571,0.585714285714286,0.6,0.614285714285714,0.628571428571428,
0.642857142857142,0.657142857142857,0.671428571428571,0.685714285714285,
0.699999999999999,0.714285714285714,0.728571428571428,0.742857142857142,
0.757142857142856,0.771428571428571,0.785714285714285,0.799999999999999,
0.814285714285713,0.828571428571428,0.842857142857142,0.857142857142856,
0.87142857142857,0.885714285714284,0.899999999999999,0.914285714285713,
0.928571428571427,0.942857142857141,0.957142857142856,0.97142857142857,
1.),.UNSPECIFIED.);
#178=B_SPLINE_CURVE_WITH_KNOTS('',3,(#17444,#17445,#17446,#17447,#17448,
#17449,#17450,#17451,#17452,#17453,#17454,#17455,#17456,#17457,#17458,#17459,
#17460,#17461,#17462,#17463,#17464,#17465,#17466,#17467,#17468,#17469,#17470,
#17471,#17472,#17473,#17474,#17475,#17476,#17477,#17478,#17479,#17480,#17481,
#17482,#17483,#17484,#17485,#17486,#17487,#17488,#17489,#17490,#17491,#17492,
#17493,#17494,#17495,#17496,#17497,#17498,#17499,#17500,#17501,#17502,#17503,
#17504,#17505,#17506,#17507,#17508,#17509,#17510,#17511,#17512,#17513),
 .UNSPECIFIED.,.F.,.F.,(4,3,3,3,3,3,3,3,3,3,3,3,3,3,3,3,3,3,3,3,3,3,3,4),
(-0.411449009780156,-0.40550489541351,-0.398537948778872,-0.388735121435802,
-0.382214695237718,-0.375350877814336,-0.367728232837723,-0.356236725561544,
-0.347888396755939,-0.337683279648765,-0.326660059466727,-0.316483474375939,
-0.302658061023146,-0.289316835726674,-0.271192407480734,-0.255261428970096,
-0.231775298750333,-0.202135573344553,-0.161986280154224,-0.126192133975022,
-0.0754619861897902,-0.0360560078842204,-0.00196685499849691,0.),
 .UNSPECIFIED.);
#179=B_SPLINE_CURVE_WITH_KNOTS('',5,(#17665,#17666,#17667,#17668,#17669,
#17670,#17671,#17672,#17673,#17674,#17675,#17676,#17677,#17678,#17679,#17680,
#17681,#17682,#17683,#17684,#17685,#17686,#17687,#17688,#17689,#17690,#17691,
#17692,#17693,#17694,#17695,#17696,#17697,#17698,#17699,#17700,#17701,#17702,
#17703,#17704,#17705,#17706,#17707,#17708,#17709,#17710,#17711,#17712,#17713,
#17714,#17715,#17716,#17717,#17718,#17719,#17720,#17721,#17722,#17723,#17724,
#17725,#17726,#17727,#17728,#17729,#17730,#17731,#17732,#17733,#17734,#17735,
#17736,#17737,#17738),.UNSPECIFIED.,.F.,.F.,(6,1,1,1,1,1,1,1,1,1,1,1,1,
1,1,1,1,1,1,1,1,1,1,1,1,1,1,1,1,1,1,1,1,1,1,1,1,1,1,1,1,1,1,1,1,1,1,1,1,
1,1,1,1,1,1,1,1,1,1,1,1,1,1,1,1,1,1,1,1,6),(0.,0.0142857142857143,0.0285714285714286,
0.0428571428571429,0.0571428571428571,0.0714285714285714,0.0857142857142857,
0.1,0.114285714285714,0.128571428571429,0.142857142857143,0.157142857142857,
0.171428571428571,0.185714285714286,0.2,0.214285714285714,0.228571428571429,
0.242857142857143,0.257142857142857,0.271428571428571,0.285714285714286,
0.3,0.314285714285714,0.328571428571429,0.342857142857143,0.357142857142857,
0.371428571428571,0.385714285714286,0.4,0.414285714285714,0.428571428571429,
0.442857142857143,0.457142857142857,0.471428571428572,0.485714285714286,
0.5,0.514285714285714,0.528571428571429,0.542857142857143,0.557142857142857,
0.571428571428571,0.585714285714286,0.6,0.614285714285714,0.628571428571428,
0.642857142857142,0.657142857142857,0.671428571428571,0.685714285714285,
0.699999999999999,0.714285714285714,0.728571428571428,0.742857142857142,
0.757142857142856,0.771428571428571,0.785714285714285,0.799999999999999,
0.814285714285713,0.828571428571428,0.842857142857142,0.857142857142856,
0.87142857142857,0.885714285714284,0.899999999999999,0.914285714285713,
0.928571428571427,0.942857142857141,0.957142857142856,0.97142857142857,
1.),.UNSPECIFIED.);
#180=B_SPLINE_CURVE_WITH_KNOTS('',3,(#17740,#17741,#17742,#17743,#17744,
#17745,#17746,#17747,#17748,#17749,#17750,#17751,#17752,#17753,#17754,#17755,
#17756,#17757,#17758,#17759,#17760,#17761,#17762,#17763,#17764,#17765,#17766,
#17767,#17768,#17769,#17770,#17771,#17772,#17773,#17774,#17775,#17776,#17777,
#17778,#17779,#17780,#17781,#17782,#17783,#17784,#17785,#17786,#17787,#17788,
#17789,#17790,#17791,#17792,#17793,#17794,#17795,#17796,#17797,#17798,#17799,
#17800,#17801,#17802,#17803,#17804,#17805,#17806),.UNSPECIFIED.,.F.,.F.,
(4,3,3,3,3,3,3,3,3,3,3,3,3,3,3,3,3,3,3,3,3,3,4),(-0.0308474254356243,-0.0282443139231585,
-0.0239308456686803,-0.0206152610248062,-0.0170461143320954,-0.0150701375499139,
-0.0131660090736057,-0.011520257939405,-0.0103391768235893,-0.00917732810571033,
-0.00816993701950823,-0.00725747185266823,-0.00648885938409023,-0.00537659348121548,
-0.00470451929606354,-0.00408467782751111,-0.00323202309648034,-0.00269108370976756,
-0.0022056157890913,-0.00169529231892506,-0.000847646159462529,-0.000380223901454506,
0.),.UNSPECIFIED.);
#181=B_SPLINE_CURVE_WITH_KNOTS('',5,(#17964,#17965,#17966,#17967,#17968,
#17969,#17970,#17971,#17972,#17973,#17974,#17975,#17976,#17977,#17978,#17979,
#17980,#17981,#17982,#17983,#17984,#17985,#17986,#17987,#17988,#17989,#17990,
#17991,#17992,#17993,#17994,#17995,#17996,#17997,#17998,#17999,#18000,#18001,
#18002,#18003,#18004,#18005,#18006,#18007,#18008,#18009,#18010,#18011,#18012,
#18013,#18014,#18015,#18016,#18017,#18018,#18019,#18020,#18021,#18022,#18023,
#18024,#18025,#18026,#18027,#18028,#18029,#18030,#18031,#18032,#18033,#18034,
#18035,#18036,#18037),.UNSPECIFIED.,.F.,.F.,(6,1,1,1,1,1,1,1,1,1,1,1,1,
1,1,1,1,1,1,1,1,1,1,1,1,1,1,1,1,1,1,1,1,1,1,1,1,1,1,1,1,1,1,1,1,1,1,1,1,
1,1,1,1,1,1,1,1,1,1,1,1,1,1,1,1,1,1,1,1,6),(0.,0.0142857142857143,0.0285714285714286,
0.0428571428571429,0.0571428571428571,0.0714285714285714,0.0857142857142857,
0.1,0.114285714285714,0.128571428571429,0.142857142857143,0.157142857142857,
0.171428571428571,0.185714285714286,0.2,0.214285714285714,0.228571428571429,
0.242857142857143,0.257142857142857,0.271428571428571,0.285714285714286,
0.3,0.314285714285714,0.328571428571429,0.342857142857143,0.357142857142857,
0.371428571428571,0.385714285714286,0.4,0.414285714285714,0.428571428571429,
0.442857142857143,0.457142857142857,0.471428571428572,0.485714285714286,
0.5,0.514285714285714,0.528571428571429,0.542857142857143,0.557142857142857,
0.571428571428571,0.585714285714286,0.6,0.614285714285714,0.628571428571428,
0.642857142857142,0.657142857142857,0.671428571428571,0.685714285714285,
0.699999999999999,0.714285714285714,0.728571428571428,0.742857142857142,
0.757142857142856,0.771428571428571,0.785714285714285,0.799999999999999,
0.814285714285713,0.828571428571428,0.842857142857142,0.857142857142856,
0.87142857142857,0.885714285714284,0.899999999999999,0.914285714285713,
0.928571428571427,0.942857142857141,0.957142857142856,0.97142857142857,
1.),.UNSPECIFIED.);
#182=B_SPLINE_CURVE_WITH_KNOTS('',3,(#18038,#18039,#18040,#18041,#18042,
#18043,#18044,#18045,#18046,#18047,#18048,#18049,#18050,#18051,#18052,#18053,
#18054,#18055,#18056,#18057,#18058,#18059,#18060,#18061,#18062,#18063,#18064,
#18065,#18066,#18067,#18068,#18069,#18070,#18071,#18072,#18073,#18074,#18075,
#18076,#18077,#18078,#18079,#18080,#18081,#18082,#18083,#18084,#18085,#18086,
#18087,#18088,#18089,#18090,#18091,#18092,#18093,#18094,#18095,#18096,#18097,
#18098,#18099,#18100,#18101,#18102,#18103,#18104,#18105,#18106,#18107),
 .UNSPECIFIED.,.F.,.F.,(4,3,3,3,3,3,3,3,3,3,3,3,3,3,3,3,3,3,3,3,3,3,3,4),
(-0.411449009963507,-0.40550489558343,-0.398537948945618,-0.388735121610794,
-0.382214695410633,-0.375350877984368,-0.367728233004637,-0.356236725723242,
-0.347888396914042,-0.337683279795922,-0.326660059606393,-0.316483474513951,
-0.302658061166432,-0.289316835878854,-0.27119240761099,-0.255261429176367,
-0.231775298979734,-0.202135573634019,-0.1619862806212,-0.126192134288906,
-0.0754619859378416,-0.0360560139109727,-0.0019668740044922,0.),
 .UNSPECIFIED.);
#183=B_SPLINE_CURVE_WITH_KNOTS('',5,(#18259,#18260,#18261,#18262,#18263,
#18264,#18265,#18266,#18267,#18268,#18269,#18270,#18271,#18272,#18273,#18274,
#18275,#18276,#18277,#18278,#18279,#18280,#18281,#18282,#18283,#18284,#18285,
#18286,#18287,#18288,#18289,#18290,#18291,#18292,#18293,#18294,#18295,#18296,
#18297,#18298,#18299,#18300,#18301,#18302,#18303,#18304,#18305,#18306,#18307,
#18308,#18309,#18310,#18311,#18312,#18313,#18314,#18315,#18316,#18317,#18318,
#18319,#18320,#18321,#18322,#18323,#18324,#18325,#18326,#18327,#18328,#18329,
#18330,#18331,#18332),.UNSPECIFIED.,.F.,.F.,(6,1,1,1,1,1,1,1,1,1,1,1,1,
1,1,1,1,1,1,1,1,1,1,1,1,1,1,1,1,1,1,1,1,1,1,1,1,1,1,1,1,1,1,1,1,1,1,1,1,
1,1,1,1,1,1,1,1,1,1,1,1,1,1,1,1,1,1,1,1,6),(0.,0.0142857142857143,0.0285714285714286,
0.0428571428571429,0.0571428571428571,0.0714285714285714,0.0857142857142857,
0.1,0.114285714285714,0.128571428571429,0.142857142857143,0.157142857142857,
0.171428571428571,0.185714285714286,0.2,0.214285714285714,0.228571428571429,
0.242857142857143,0.257142857142857,0.271428571428571,0.285714285714286,
0.3,0.314285714285714,0.328571428571429,0.342857142857143,0.357142857142857,
0.371428571428571,0.385714285714286,0.4,0.414285714285714,0.428571428571429,
0.442857142857143,0.457142857142857,0.471428571428572,0.485714285714286,
0.5,0.514285714285714,0.528571428571429,0.542857142857143,0.557142857142857,
0.571428571428571,0.585714285714286,0.6,0.614285714285714,0.628571428571428,
0.642857142857142,0.657142857142857,0.671428571428571,0.685714285714285,
0.699999999999999,0.714285714285714,0.728571428571428,0.742857142857142,
0.757142857142856,0.771428571428571,0.785714285714285,0.799999999999999,
0.814285714285713,0.828571428571428,0.842857142857142,0.857142857142856,
0.87142857142857,0.885714285714284,0.899999999999999,0.914285714285713,
0.928571428571427,0.942857142857141,0.957142857142856,0.97142857142857,
1.),.UNSPECIFIED.);
#184=B_SPLINE_CURVE_WITH_KNOTS('',3,(#18334,#18335,#18336,#18337,#18338,
#18339,#18340,#18341,#18342,#18343,#18344,#18345,#18346,#18347,#18348,#18349,
#18350,#18351,#18352,#18353,#18354,#18355,#18356,#18357,#18358,#18359,#18360,
#18361,#18362,#18363,#18364,#18365,#18366,#18367,#18368,#18369,#18370,#18371,
#18372,#18373,#18374,#18375,#18376,#18377,#18378,#18379,#18380,#18381,#18382,
#18383,#18384,#18385,#18386,#18387,#18388,#18389,#18390,#18391,#18392,#18393,
#18394,#18395,#18396,#18397,#18398,#18399,#18400),.UNSPECIFIED.,.F.,.F.,
(4,3,3,3,3,3,3,3,3,3,3,3,3,3,3,3,3,3,3,3,3,3,4),(-0.030847425423351,-0.0282443142621516,
-0.0239308460522739,-0.0206152614247573,-0.0170461144001592,-0.0150701376854405,
-0.0131660090123514,-0.0115202578858075,-0.0103391767661309,-0.00917732807723113,
-0.00816993700701968,-0.0072574718323543,-0.00648885936596464,-0.00537659349330486,
-0.00470451930664176,-0.00408467783955803,-0.00323202308982742,-0.00269108370404856,
-0.00220561578379538,-0.00169529231302908,-0.000847646156514541,-0.000380223899127519,
0.),.UNSPECIFIED.);
#185=B_SPLINE_CURVE_WITH_KNOTS('',5,(#18558,#18559,#18560,#18561,#18562,
#18563,#18564,#18565,#18566,#18567,#18568,#18569,#18570,#18571,#18572,#18573,
#18574,#18575,#18576,#18577,#18578,#18579,#18580,#18581,#18582,#18583,#18584,
#18585,#18586,#18587,#18588,#18589,#18590,#18591,#18592,#18593,#18594,#18595,
#18596,#18597,#18598,#18599,#18600,#18601,#18602,#18603,#18604,#18605,#18606,
#18607,#18608,#18609,#18610,#18611,#18612,#18613,#18614,#18615,#18616,#18617,
#18618,#18619,#18620,#18621,#18622,#18623,#18624,#18625,#18626,#18627,#18628,
#18629,#18630,#18631),.UNSPECIFIED.,.F.,.F.,(6,1,1,1,1,1,1,1,1,1,1,1,1,
1,1,1,1,1,1,1,1,1,1,1,1,1,1,1,1,1,1,1,1,1,1,1,1,1,1,1,1,1,1,1,1,1,1,1,1,
1,1,1,1,1,1,1,1,1,1,1,1,1,1,1,1,1,1,1,1,6),(0.,0.0142857142857143,0.0285714285714286,
0.0428571428571429,0.0571428571428571,0.0714285714285714,0.0857142857142857,
0.1,0.114285714285714,0.128571428571429,0.142857142857143,0.157142857142857,
0.171428571428571,0.185714285714286,0.2,0.214285714285714,0.228571428571429,
0.242857142857143,0.257142857142857,0.271428571428571,0.285714285714286,
0.3,0.314285714285714,0.328571428571429,0.342857142857143,0.357142857142857,
0.371428571428571,0.385714285714286,0.4,0.414285714285714,0.428571428571429,
0.442857142857143,0.457142857142857,0.471428571428572,0.485714285714286,
0.5,0.514285714285714,0.528571428571429,0.542857142857143,0.557142857142857,
0.571428571428571,0.585714285714286,0.6,0.614285714285714,0.628571428571428,
0.642857142857142,0.657142857142857,0.671428571428571,0.685714285714285,
0.699999999999999,0.714285714285714,0.728571428571428,0.742857142857142,
0.757142857142856,0.771428571428571,0.785714285714285,0.799999999999999,
0.814285714285713,0.828571428571428,0.842857142857142,0.857142857142856,
0.87142857142857,0.885714285714284,0.899999999999999,0.914285714285713,
0.928571428571427,0.942857142857141,0.957142857142856,0.97142857142857,
1.),.UNSPECIFIED.);
#186=B_SPLINE_CURVE_WITH_KNOTS('',3,(#18632,#18633,#18634,#18635,#18636,
#18637,#18638,#18639,#18640,#18641,#18642,#18643,#18644,#18645,#18646,#18647,
#18648,#18649,#18650,#18651,#18652,#18653,#18654,#18655,#18656,#18657,#18658,
#18659,#18660,#18661,#18662,#18663,#18664,#18665,#18666,#18667,#18668,#18669,
#18670,#18671,#18672,#18673,#18674,#18675,#18676,#18677,#18678,#18679,#18680,
#18681,#18682,#18683,#18684,#18685,#18686,#18687,#18688,#18689,#18690,#18691,
#18692,#18693,#18694,#18695,#18696,#18697,#18698,#18699,#18700,#18701),
 .UNSPECIFIED.,.F.,.F.,(4,3,3,3,3,3,3,3,3,3,3,3,3,3,3,3,3,3,3,3,3,3,3,4),
(-0.411449009976945,-0.405504895592072,-0.398537948953833,-0.388735121623208,
-0.382214695422447,-0.375350877996945,-0.367728233016586,-0.356236725734817,
-0.347888396925664,-0.337683279812359,-0.326660059622673,-0.31648347452754,
-0.302658061159068,-0.289316835870757,-0.271192407500547,-0.255261428976667,
-0.231775298862027,-0.202135573483824,-0.16198628029512,-0.126192133881173,
-0.0754619854549211,-0.0360560096240121,-0.00196686195736208,0.),
 .UNSPECIFIED.);
#187=B_SPLINE_CURVE_WITH_KNOTS('',5,(#18727,#18728,#18729,#18730,#18731,
#18732,#18733,#18734,#18735,#18736,#18737,#18738,#18739,#18740,#18741,#18742,
#18743,#18744,#18745,#18746,#18747,#18748,#18749,#18750,#18751,#18752,#18753,
#18754,#18755,#18756,#18757,#18758,#18759,#18760,#18761,#18762,#18763,#18764,
#18765,#18766,#18767,#18768,#18769,#18770,#18771,#18772,#18773,#18774,#18775,
#18776,#18777,#18778,#18779,#18780,#18781,#18782,#18783,#18784,#18785,#18786,
#18787,#18788,#18789,#18790,#18791,#18792,#18793,#18794,#18795,#18796,#18797,
#18798,#18799,#18800),.UNSPECIFIED.,.F.,.F.,(6,1,1,1,1,1,1,1,1,1,1,1,1,
1,1,1,1,1,1,1,1,1,1,1,1,1,1,1,1,1,1,1,1,1,1,1,1,1,1,1,1,1,1,1,1,1,1,1,1,
1,1,1,1,1,1,1,1,1,1,1,1,1,1,1,1,1,1,1,1,6),(0.,0.0142857142857143,0.0285714285714286,
0.0428571428571429,0.0571428571428571,0.0714285714285714,0.0857142857142857,
0.1,0.114285714285714,0.128571428571429,0.142857142857143,0.157142857142857,
0.171428571428571,0.185714285714286,0.2,0.214285714285714,0.228571428571429,
0.242857142857143,0.257142857142857,0.271428571428571,0.285714285714286,
0.3,0.314285714285714,0.328571428571429,0.342857142857143,0.357142857142857,
0.371428571428571,0.385714285714286,0.4,0.414285714285714,0.428571428571429,
0.442857142857143,0.457142857142857,0.471428571428572,0.485714285714286,
0.5,0.514285714285714,0.528571428571429,0.542857142857143,0.557142857142857,
0.571428571428571,0.585714285714286,0.6,0.614285714285714,0.628571428571428,
0.642857142857142,0.657142857142857,0.671428571428571,0.685714285714285,
0.699999999999999,0.714285714285714,0.728571428571428,0.742857142857142,
0.757142857142856,0.771428571428571,0.785714285714285,0.799999999999999,
0.814285714285713,0.828571428571428,0.842857142857142,0.857142857142856,
0.87142857142857,0.885714285714284,0.899999999999999,0.914285714285713,
0.928571428571427,0.942857142857141,0.957142857142856,0.97142857142857,
1.),.UNSPECIFIED.);
#188=B_SPLINE_CURVE_WITH_KNOTS('',5,(#18804,#18805,#18806,#18807,#18808,
#18809,#18810,#18811,#18812,#18813,#18814,#18815,#18816,#18817,#18818,#18819,
#18820,#18821,#18822,#18823,#18824,#18825,#18826,#18827,#18828,#18829,#18830,
#18831,#18832,#18833,#18834,#18835,#18836,#18837,#18838,#18839,#18840,#18841,
#18842,#18843,#18844,#18845,#18846,#18847,#18848,#18849,#18850,#18851,#18852,
#18853,#18854,#18855,#18856,#18857,#18858,#18859,#18860,#18861,#18862,#18863,
#18864,#18865,#18866,#18867,#18868,#18869,#18870,#18871,#18872,#18873,#18874,
#18875,#18876,#18877),.UNSPECIFIED.,.F.,.F.,(6,1,1,1,1,1,1,1,1,1,1,1,1,
1,1,1,1,1,1,1,1,1,1,1,1,1,1,1,1,1,1,1,1,1,1,1,1,1,1,1,1,1,1,1,1,1,1,1,1,
1,1,1,1,1,1,1,1,1,1,1,1,1,1,1,1,1,1,1,1,6),(0.,0.0142857142857143,0.0285714285714286,
0.0428571428571429,0.0571428571428571,0.0714285714285714,0.0857142857142857,
0.1,0.114285714285714,0.128571428571429,0.142857142857143,0.157142857142857,
0.171428571428571,0.185714285714286,0.2,0.214285714285714,0.228571428571429,
0.242857142857143,0.257142857142857,0.271428571428571,0.285714285714286,
0.3,0.314285714285714,0.328571428571429,0.342857142857143,0.357142857142857,
0.371428571428571,0.385714285714286,0.4,0.414285714285714,0.428571428571429,
0.442857142857143,0.457142857142857,0.471428571428572,0.485714285714286,
0.5,0.514285714285714,0.528571428571429,0.542857142857143,0.557142857142857,
0.571428571428571,0.585714285714286,0.6,0.614285714285714,0.628571428571428,
0.642857142857142,0.657142857142857,0.671428571428571,0.685714285714285,
0.699999999999999,0.714285714285714,0.728571428571428,0.742857142857142,
0.757142857142856,0.771428571428571,0.785714285714285,0.799999999999999,
0.814285714285713,0.828571428571428,0.842857142857142,0.857142857142856,
0.87142857142857,0.885714285714284,0.899999999999999,0.914285714285713,
0.928571428571427,0.942857142857141,0.957142857142856,0.97142857142857,
1.),.UNSPECIFIED.);
#189=B_SPLINE_CURVE_WITH_KNOTS('',3,(#18892,#18893,#18894,#18895,#18896,
#18897,#18898,#18899,#18900,#18901,#18902,#18903,#18904,#18905,#18906,#18907,
#18908,#18909,#18910,#18911,#18912,#18913,#18914,#18915,#18916,#18917,#18918,
#18919,#18920,#18921,#18922,#18923,#18924,#18925,#18926,#18927,#18928,#18929,
#18930,#18931,#18932,#18933,#18934,#18935,#18936,#18937,#18938,#18939,#18940,
#18941,#18942,#18943,#18944,#18945,#18946,#18947,#18948,#18949,#18950,#18951,
#18952,#18953,#18954,#18955,#18956,#18957,#18958,#18959,#18960,#18961),
 .UNSPECIFIED.,.F.,.F.,(4,3,3,3,3,3,3,3,3,3,3,3,3,3,3,3,3,3,3,3,3,3,3,4),
(-0.411449009793068,-0.405504895416512,-0.398537948781067,-0.38873512144739,
-0.382214695249858,-0.375350877826228,-0.367728232848294,-0.356236725571785,
-0.347888396766066,-0.33768327965463,-0.326660059470826,-0.316483474377544,
-0.302658061011095,-0.289316835715289,-0.271192407328683,-0.255261428798271,
-0.23177529872749,-0.202135573370612,-0.161986280260425,-0.126192134080337,
-0.075461985655617,-0.0360560111852818,-0.00196686554572469,0.),
 .UNSPECIFIED.);
#190=B_SPLINE_CURVE_WITH_KNOTS('',3,(#18965,#18966,#18967,#18968,#18969,
#18970,#18971,#18972,#18973,#18974,#18975,#18976,#18977,#18978,#18979,#18980,
#18981,#18982,#18983,#18984,#18985,#18986,#18987,#18988,#18989,#18990,#18991,
#18992,#18993,#18994,#18995,#18996,#18997,#18998,#18999,#19000,#19001,#19002,
#19003,#19004,#19005,#19006,#19007,#19008,#19009,#19010,#19011,#19012,#19013,
#19014,#19015,#19016,#19017,#19018,#19019,#19020,#19021,#19022,#19023,#19024,
#19025,#19026,#19027,#19028,#19029,#19030,#19031),.UNSPECIFIED.,.F.,.F.,
(4,3,3,3,3,3,3,3,3,3,3,3,3,3,3,3,3,3,3,3,3,3,4),(-0.03084742543048,-0.0282443142384382,
-0.0239308460027108,-0.0206152613738073,-0.0170461144147563,-0.0150701377170469,
-0.0131660090069468,-0.0115202578810785,-0.0103391767598669,-0.00917732807488943,
-0.00816993700694134,-0.00725747182913227,-0.00648885936321739,-0.00537659349882703,
-0.00470451931147365,-0.00408467784459405,-0.00323202308945096,-0.00269108370363151,
-0.00220561578335159,-0.00169529231220793,-0.000847646156103964,-0.000380223898199378,
0.),.UNSPECIFIED.);
#191=B_SPLINE_SURFACE_WITH_KNOTS('',5,1,((#7395,#7396),(#7397,#7398),(#7399,
#7400),(#7401,#7402),(#7403,#7404),(#7405,#7406),(#7407,#7408),(#7409,#7410),
(#7411,#7412),(#7413,#7414),(#7415,#7416),(#7417,#7418),(#7419,#7420),(#7421,
#7422),(#7423,#7424),(#7425,#7426),(#7427,#7428),(#7429,#7430),(#7431,#7432),
(#7433,#7434),(#7435,#7436),(#7437,#7438),(#7439,#7440),(#7441,#7442),(#7443,
#7444),(#7445,#7446),(#7447,#7448),(#7449,#7450),(#7451,#7452),(#7453,#7454),
(#7455,#7456),(#7457,#7458),(#7459,#7460),(#7461,#7462),(#7463,#7464),(#7465,
#7466),(#7467,#7468),(#7469,#7470),(#7471,#7472),(#7473,#7474),(#7475,#7476),
(#7477,#7478),(#7479,#7480),(#7481,#7482),(#7483,#7484),(#7485,#7486),(#7487,
#7488),(#7489,#7490),(#7491,#7492),(#7493,#7494),(#7495,#7496),(#7497,#7498),
(#7499,#7500),(#7501,#7502),(#7503,#7504),(#7505,#7506),(#7507,#7508),(#7509,
#7510),(#7511,#7512),(#7513,#7514),(#7515,#7516),(#7517,#7518),(#7519,#7520),
(#7521,#7522),(#7523,#7524),(#7525,#7526),(#7527,#7528),(#7529,#7530),(#7531,
#7532),(#7533,#7534),(#7535,#7536),(#7537,#7538),(#7539,#7540),(#7541,#7542),
(#7543,#7544)),.UNSPECIFIED.,.F.,.F.,.F.,(6,1,1,1,1,1,1,1,1,1,1,1,1,1,1,
1,1,1,1,1,1,1,1,1,1,1,1,1,1,1,1,1,1,1,1,1,1,1,1,1,1,1,1,1,1,1,1,1,1,1,1,
1,1,1,1,1,1,1,1,1,1,1,1,1,1,1,1,1,1,1,6),(2,2),(-1.,-0.985714285714284,
-0.97142857142857,-0.957142857142856,-0.942857142857141,-0.928571428571427,
-0.914285714285713,-0.899999999999999,-0.885714285714284,-0.87142857142857,
-0.857142857142856,-0.842857142857142,-0.828571428571428,-0.814285714285713,
-0.799999999999999,-0.785714285714285,-0.771428571428571,-0.757142857142856,
-0.742857142857142,-0.728571428571428,-0.714285714285714,-0.699999999999999,
-0.685714285714285,-0.671428571428571,-0.657142857142857,-0.642857142857142,
-0.628571428571428,-0.614285714285714,-0.6,-0.585714285714286,-0.571428571428571,
-0.557142857142857,-0.542857142857143,-0.528571428571429,-0.514285714285714,
-0.5,-0.485714285714286,-0.471428571428572,-0.457142857142857,-0.442857142857143,
-0.428571428571429,-0.414285714285714,-0.4,-0.385714285714286,-0.371428571428571,
-0.357142857142857,-0.342857142857143,-0.328571428571429,-0.314285714285714,
-0.3,-0.285714285714286,-0.271428571428571,-0.257142857142857,-0.242857142857143,
-0.228571428571429,-0.214285714285714,-0.2,-0.185714285714286,-0.171428571428571,
-0.157142857142857,-0.142857142857143,-0.128571428571429,-0.114285714285714,
-0.1,-0.0857142857142857,-0.0714285714285714,-0.0571428571428571,-0.0428571428571429,
-0.0285714285714286,-0.0142857142857143,0.),(0.,2.1),.UNSPECIFIED.);
#192=B_SPLINE_SURFACE_WITH_KNOTS('',5,1,((#7695,#7696),(#7697,#7698),(#7699,
#7700),(#7701,#7702),(#7703,#7704),(#7705,#7706),(#7707,#7708),(#7709,#7710),
(#7711,#7712),(#7713,#7714),(#7715,#7716),(#7717,#7718),(#7719,#7720),(#7721,
#7722),(#7723,#7724),(#7725,#7726),(#7727,#7728),(#7729,#7730),(#7731,#7732),
(#7733,#7734),(#7735,#7736),(#7737,#7738),(#7739,#7740),(#7741,#7742),(#7743,
#7744),(#7745,#7746),(#7747,#7748),(#7749,#7750),(#7751,#7752),(#7753,#7754),
(#7755,#7756),(#7757,#7758),(#7759,#7760),(#7761,#7762),(#7763,#7764),(#7765,
#7766),(#7767,#7768),(#7769,#7770),(#7771,#7772),(#7773,#7774),(#7775,#7776),
(#7777,#7778),(#7779,#7780),(#7781,#7782),(#7783,#7784),(#7785,#7786),(#7787,
#7788),(#7789,#7790),(#7791,#7792),(#7793,#7794),(#7795,#7796),(#7797,#7798),
(#7799,#7800),(#7801,#7802),(#7803,#7804),(#7805,#7806),(#7807,#7808),(#7809,
#7810),(#7811,#7812),(#7813,#7814),(#7815,#7816),(#7817,#7818),(#7819,#7820),
(#7821,#7822),(#7823,#7824),(#7825,#7826),(#7827,#7828),(#7829,#7830),(#7831,
#7832),(#7833,#7834),(#7835,#7836),(#7837,#7838),(#7839,#7840),(#7841,#7842),
(#7843,#7844)),.UNSPECIFIED.,.F.,.F.,.F.,(6,1,1,1,1,1,1,1,1,1,1,1,1,1,1,
1,1,1,1,1,1,1,1,1,1,1,1,1,1,1,1,1,1,1,1,1,1,1,1,1,1,1,1,1,1,1,1,1,1,1,1,
1,1,1,1,1,1,1,1,1,1,1,1,1,1,1,1,1,1,1,6),(2,2),(0.,0.0142857142857143,0.0285714285714286,
0.0428571428571429,0.0571428571428571,0.0714285714285714,0.0857142857142857,
0.1,0.114285714285714,0.128571428571429,0.142857142857143,0.157142857142857,
0.171428571428571,0.185714285714286,0.2,0.214285714285714,0.228571428571429,
0.242857142857143,0.257142857142857,0.271428571428571,0.285714285714286,
0.3,0.314285714285714,0.328571428571429,0.342857142857143,0.357142857142857,
0.371428571428571,0.385714285714286,0.4,0.414285714285714,0.428571428571429,
0.442857142857143,0.457142857142857,0.471428571428572,0.485714285714286,
0.5,0.514285714285714,0.528571428571429,0.542857142857143,0.557142857142857,
0.571428571428571,0.585714285714286,0.6,0.614285714285714,0.628571428571428,
0.642857142857142,0.657142857142857,0.671428571428571,0.685714285714285,
0.699999999999999,0.714285714285714,0.728571428571428,0.742857142857142,
0.757142857142856,0.771428571428571,0.785714285714285,0.799999999999999,
0.814285714285713,0.828571428571428,0.842857142857142,0.857142857142856,
0.87142857142857,0.885714285714284,0.899999999999999,0.914285714285713,
0.928571428571427,0.942857142857141,0.957142857142856,0.97142857142857,
0.985714285714284,1.),(0.,2.1),.UNSPECIFIED.);
#193=B_SPLINE_SURFACE_WITH_KNOTS('',5,1,((#7989,#7990),(#7991,#7992),(#7993,
#7994),(#7995,#7996),(#7997,#7998),(#7999,#8000),(#8001,#8002),(#8003,#8004),
(#8005,#8006),(#8007,#8008),(#8009,#8010),(#8011,#8012),(#8013,#8014),(#8015,
#8016),(#8017,#8018),(#8019,#8020),(#8021,#8022),(#8023,#8024),(#8025,#8026),
(#8027,#8028),(#8029,#8030),(#8031,#8032),(#8033,#8034),(#8035,#8036),(#8037,
#8038),(#8039,#8040),(#8041,#8042),(#8043,#8044),(#8045,#8046),(#8047,#8048),
(#8049,#8050),(#8051,#8052),(#8053,#8054),(#8055,#8056),(#8057,#8058),(#8059,
#8060),(#8061,#8062),(#8063,#8064),(#8065,#8066),(#8067,#8068),(#8069,#8070),
(#8071,#8072),(#8073,#8074),(#8075,#8076),(#8077,#8078),(#8079,#8080),(#8081,
#8082),(#8083,#8084),(#8085,#8086),(#8087,#8088),(#8089,#8090),(#8091,#8092),
(#8093,#8094),(#8095,#8096),(#8097,#8098),(#8099,#8100),(#8101,#8102),(#8103,
#8104),(#8105,#8106),(#8107,#8108),(#8109,#8110),(#8111,#8112),(#8113,#8114),
(#8115,#8116),(#8117,#8118),(#8119,#8120),(#8121,#8122),(#8123,#8124),(#8125,
#8126),(#8127,#8128),(#8129,#8130),(#8131,#8132),(#8133,#8134),(#8135,#8136),
(#8137,#8138)),.UNSPECIFIED.,.F.,.F.,.F.,(6,1,1,1,1,1,1,1,1,1,1,1,1,1,1,
1,1,1,1,1,1,1,1,1,1,1,1,1,1,1,1,1,1,1,1,1,1,1,1,1,1,1,1,1,1,1,1,1,1,1,1,
1,1,1,1,1,1,1,1,1,1,1,1,1,1,1,1,1,1,1,6),(2,2),(-1.,-0.985714285714284,
-0.97142857142857,-0.957142857142856,-0.942857142857141,-0.928571428571427,
-0.914285714285713,-0.899999999999999,-0.885714285714284,-0.87142857142857,
-0.857142857142856,-0.842857142857142,-0.828571428571428,-0.814285714285713,
-0.799999999999999,-0.785714285714285,-0.771428571428571,-0.757142857142856,
-0.742857142857142,-0.728571428571428,-0.714285714285714,-0.699999999999999,
-0.685714285714285,-0.671428571428571,-0.657142857142857,-0.642857142857142,
-0.628571428571428,-0.614285714285714,-0.6,-0.585714285714286,-0.571428571428571,
-0.557142857142857,-0.542857142857143,-0.528571428571429,-0.514285714285714,
-0.5,-0.485714285714286,-0.471428571428572,-0.457142857142857,-0.442857142857143,
-0.428571428571429,-0.414285714285714,-0.4,-0.385714285714286,-0.371428571428571,
-0.357142857142857,-0.342857142857143,-0.328571428571429,-0.314285714285714,
-0.3,-0.285714285714286,-0.271428571428571,-0.257142857142857,-0.242857142857143,
-0.228571428571429,-0.214285714285714,-0.2,-0.185714285714286,-0.171428571428571,
-0.157142857142857,-0.142857142857143,-0.128571428571429,-0.114285714285714,
-0.1,-0.0857142857142857,-0.0714285714285714,-0.0571428571428571,-0.0428571428571429,
-0.0285714285714286,-0.0142857142857143,0.),(0.,2.1),.UNSPECIFIED.);
#194=B_SPLINE_SURFACE_WITH_KNOTS('',5,1,((#8289,#8290),(#8291,#8292),(#8293,
#8294),(#8295,#8296),(#8297,#8298),(#8299,#8300),(#8301,#8302),(#8303,#8304),
(#8305,#8306),(#8307,#8308),(#8309,#8310),(#8311,#8312),(#8313,#8314),(#8315,
#8316),(#8317,#8318),(#8319,#8320),(#8321,#8322),(#8323,#8324),(#8325,#8326),
(#8327,#8328),(#8329,#8330),(#8331,#8332),(#8333,#8334),(#8335,#8336),(#8337,
#8338),(#8339,#8340),(#8341,#8342),(#8343,#8344),(#8345,#8346),(#8347,#8348),
(#8349,#8350),(#8351,#8352),(#8353,#8354),(#8355,#8356),(#8357,#8358),(#8359,
#8360),(#8361,#8362),(#8363,#8364),(#8365,#8366),(#8367,#8368),(#8369,#8370),
(#8371,#8372),(#8373,#8374),(#8375,#8376),(#8377,#8378),(#8379,#8380),(#8381,
#8382),(#8383,#8384),(#8385,#8386),(#8387,#8388),(#8389,#8390),(#8391,#8392),
(#8393,#8394),(#8395,#8396),(#8397,#8398),(#8399,#8400),(#8401,#8402),(#8403,
#8404),(#8405,#8406),(#8407,#8408),(#8409,#8410),(#8411,#8412),(#8413,#8414),
(#8415,#8416),(#8417,#8418),(#8419,#8420),(#8421,#8422),(#8423,#8424),(#8425,
#8426),(#8427,#8428),(#8429,#8430),(#8431,#8432),(#8433,#8434),(#8435,#8436),
(#8437,#8438)),.UNSPECIFIED.,.F.,.F.,.F.,(6,1,1,1,1,1,1,1,1,1,1,1,1,1,1,
1,1,1,1,1,1,1,1,1,1,1,1,1,1,1,1,1,1,1,1,1,1,1,1,1,1,1,1,1,1,1,1,1,1,1,1,
1,1,1,1,1,1,1,1,1,1,1,1,1,1,1,1,1,1,1,6),(2,2),(0.,0.0142857142857143,0.0285714285714286,
0.0428571428571429,0.0571428571428571,0.0714285714285714,0.0857142857142857,
0.1,0.114285714285714,0.128571428571429,0.142857142857143,0.157142857142857,
0.171428571428571,0.185714285714286,0.2,0.214285714285714,0.228571428571429,
0.242857142857143,0.257142857142857,0.271428571428571,0.285714285714286,
0.3,0.314285714285714,0.328571428571429,0.342857142857143,0.357142857142857,
0.371428571428571,0.385714285714286,0.4,0.414285714285714,0.428571428571429,
0.442857142857143,0.457142857142857,0.471428571428572,0.485714285714286,
0.5,0.514285714285714,0.528571428571429,0.542857142857143,0.557142857142857,
0.571428571428571,0.585714285714286,0.6,0.614285714285714,0.628571428571428,
0.642857142857142,0.657142857142857,0.671428571428571,0.685714285714285,
0.699999999999999,0.714285714285714,0.728571428571428,0.742857142857142,
0.757142857142856,0.771428571428571,0.785714285714285,0.799999999999999,
0.814285714285713,0.828571428571428,0.842857142857142,0.857142857142856,
0.87142857142857,0.885714285714284,0.899999999999999,0.914285714285713,
0.928571428571427,0.942857142857141,0.957142857142856,0.97142857142857,
0.985714285714284,1.),(0.,2.1),.UNSPECIFIED.);
#195=B_SPLINE_SURFACE_WITH_KNOTS('',5,1,((#8589,#8590),(#8591,#8592),(#8593,
#8594),(#8595,#8596),(#8597,#8598),(#8599,#8600),(#8601,#8602),(#8603,#8604),
(#8605,#8606),(#8607,#8608),(#8609,#8610),(#8611,#8612),(#8613,#8614),(#8615,
#8616),(#8617,#8618),(#8619,#8620),(#8621,#8622),(#8623,#8624),(#8625,#8626),
(#8627,#8628),(#8629,#8630),(#8631,#8632),(#8633,#8634),(#8635,#8636),(#8637,
#8638),(#8639,#8640),(#8641,#8642),(#8643,#8644),(#8645,#8646),(#8647,#8648),
(#8649,#8650),(#8651,#8652),(#8653,#8654),(#8655,#8656),(#8657,#8658),(#8659,
#8660),(#8661,#8662),(#8663,#8664),(#8665,#8666),(#8667,#8668),(#8669,#8670),
(#8671,#8672),(#8673,#8674),(#8675,#8676),(#8677,#8678),(#8679,#8680),(#8681,
#8682),(#8683,#8684),(#8685,#8686),(#8687,#8688),(#8689,#8690),(#8691,#8692),
(#8693,#8694),(#8695,#8696),(#8697,#8698),(#8699,#8700),(#8701,#8702),(#8703,
#8704),(#8705,#8706),(#8707,#8708),(#8709,#8710),(#8711,#8712),(#8713,#8714),
(#8715,#8716),(#8717,#8718),(#8719,#8720),(#8721,#8722),(#8723,#8724),(#8725,
#8726),(#8727,#8728),(#8729,#8730),(#8731,#8732),(#8733,#8734),(#8735,#8736),
(#8737,#8738)),.UNSPECIFIED.,.F.,.F.,.F.,(6,1,1,1,1,1,1,1,1,1,1,1,1,1,1,
1,1,1,1,1,1,1,1,1,1,1,1,1,1,1,1,1,1,1,1,1,1,1,1,1,1,1,1,1,1,1,1,1,1,1,1,
1,1,1,1,1,1,1,1,1,1,1,1,1,1,1,1,1,1,1,6),(2,2),(-1.,-0.985714285714284,
-0.97142857142857,-0.957142857142856,-0.942857142857141,-0.928571428571427,
-0.914285714285713,-0.899999999999999,-0.885714285714284,-0.87142857142857,
-0.857142857142856,-0.842857142857142,-0.828571428571428,-0.814285714285713,
-0.799999999999999,-0.785714285714285,-0.771428571428571,-0.757142857142856,
-0.742857142857142,-0.728571428571428,-0.714285714285714,-0.699999999999999,
-0.685714285714285,-0.671428571428571,-0.657142857142857,-0.642857142857142,
-0.628571428571428,-0.614285714285714,-0.6,-0.585714285714286,-0.571428571428571,
-0.557142857142857,-0.542857142857143,-0.528571428571429,-0.514285714285714,
-0.5,-0.485714285714286,-0.471428571428572,-0.457142857142857,-0.442857142857143,
-0.428571428571429,-0.414285714285714,-0.4,-0.385714285714286,-0.371428571428571,
-0.357142857142857,-0.342857142857143,-0.328571428571429,-0.314285714285714,
-0.3,-0.285714285714286,-0.271428571428571,-0.257142857142857,-0.242857142857143,
-0.228571428571429,-0.214285714285714,-0.2,-0.185714285714286,-0.171428571428571,
-0.157142857142857,-0.142857142857143,-0.128571428571429,-0.114285714285714,
-0.1,-0.0857142857142857,-0.0714285714285714,-0.0571428571428571,-0.0428571428571429,
-0.0285714285714286,-0.0142857142857143,0.),(0.,2.1),.UNSPECIFIED.);
#196=B_SPLINE_SURFACE_WITH_KNOTS('',5,1,((#8889,#8890),(#8891,#8892),(#8893,
#8894),(#8895,#8896),(#8897,#8898),(#8899,#8900),(#8901,#8902),(#8903,#8904),
(#8905,#8906),(#8907,#8908),(#8909,#8910),(#8911,#8912),(#8913,#8914),(#8915,
#8916),(#8917,#8918),(#8919,#8920),(#8921,#8922),(#8923,#8924),(#8925,#8926),
(#8927,#8928),(#8929,#8930),(#8931,#8932),(#8933,#8934),(#8935,#8936),(#8937,
#8938),(#8939,#8940),(#8941,#8942),(#8943,#8944),(#8945,#8946),(#8947,#8948),
(#8949,#8950),(#8951,#8952),(#8953,#8954),(#8955,#8956),(#8957,#8958),(#8959,
#8960),(#8961,#8962),(#8963,#8964),(#8965,#8966),(#8967,#8968),(#8969,#8970),
(#8971,#8972),(#8973,#8974),(#8975,#8976),(#8977,#8978),(#8979,#8980),(#8981,
#8982),(#8983,#8984),(#8985,#8986),(#8987,#8988),(#8989,#8990),(#8991,#8992),
(#8993,#8994),(#8995,#8996),(#8997,#8998),(#8999,#9000),(#9001,#9002),(#9003,
#9004),(#9005,#9006),(#9007,#9008),(#9009,#9010),(#9011,#9012),(#9013,#9014),
(#9015,#9016),(#9017,#9018),(#9019,#9020),(#9021,#9022),(#9023,#9024),(#9025,
#9026),(#9027,#9028),(#9029,#9030),(#9031,#9032),(#9033,#9034),(#9035,#9036),
(#9037,#9038)),.UNSPECIFIED.,.F.,.F.,.F.,(6,1,1,1,1,1,1,1,1,1,1,1,1,1,1,
1,1,1,1,1,1,1,1,1,1,1,1,1,1,1,1,1,1,1,1,1,1,1,1,1,1,1,1,1,1,1,1,1,1,1,1,
1,1,1,1,1,1,1,1,1,1,1,1,1,1,1,1,1,1,1,6),(2,2),(0.,0.0142857142857143,0.0285714285714286,
0.0428571428571429,0.0571428571428571,0.0714285714285714,0.0857142857142857,
0.1,0.114285714285714,0.128571428571429,0.142857142857143,0.157142857142857,
0.171428571428571,0.185714285714286,0.2,0.214285714285714,0.228571428571429,
0.242857142857143,0.257142857142857,0.271428571428571,0.285714285714286,
0.3,0.314285714285714,0.328571428571429,0.342857142857143,0.357142857142857,
0.371428571428571,0.385714285714286,0.4,0.414285714285714,0.428571428571429,
0.442857142857143,0.457142857142857,0.471428571428572,0.485714285714286,
0.5,0.514285714285714,0.528571428571429,0.542857142857143,0.557142857142857,
0.571428571428571,0.585714285714286,0.6,0.614285714285714,0.628571428571428,
0.642857142857142,0.657142857142857,0.671428571428571,0.685714285714285,
0.699999999999999,0.714285714285714,0.728571428571428,0.742857142857142,
0.757142857142856,0.771428571428571,0.785714285714285,0.799999999999999,
0.814285714285713,0.828571428571428,0.842857142857142,0.857142857142856,
0.87142857142857,0.885714285714284,0.899999999999999,0.914285714285713,
0.928571428571427,0.942857142857141,0.957142857142856,0.97142857142857,
0.985714285714284,1.),(0.,2.1),.UNSPECIFIED.);
#197=B_SPLINE_SURFACE_WITH_KNOTS('',5,1,((#9183,#9184),(#9185,#9186),(#9187,
#9188),(#9189,#9190),(#9191,#9192),(#9193,#9194),(#9195,#9196),(#9197,#9198),
(#9199,#9200),(#9201,#9202),(#9203,#9204),(#9205,#9206),(#9207,#9208),(#9209,
#9210),(#9211,#9212),(#9213,#9214),(#9215,#9216),(#9217,#9218),(#9219,#9220),
(#9221,#9222),(#9223,#9224),(#9225,#9226),(#9227,#9228),(#9229,#9230),(#9231,
#9232),(#9233,#9234),(#9235,#9236),(#9237,#9238),(#9239,#9240),(#9241,#9242),
(#9243,#9244),(#9245,#9246),(#9247,#9248),(#9249,#9250),(#9251,#9252),(#9253,
#9254),(#9255,#9256),(#9257,#9258),(#9259,#9260),(#9261,#9262),(#9263,#9264),
(#9265,#9266),(#9267,#9268),(#9269,#9270),(#9271,#9272),(#9273,#9274),(#9275,
#9276),(#9277,#9278),(#9279,#9280),(#9281,#9282),(#9283,#9284),(#9285,#9286),
(#9287,#9288),(#9289,#9290),(#9291,#9292),(#9293,#9294),(#9295,#9296),(#9297,
#9298),(#9299,#9300),(#9301,#9302),(#9303,#9304),(#9305,#9306),(#9307,#9308),
(#9309,#9310),(#9311,#9312),(#9313,#9314),(#9315,#9316),(#9317,#9318),(#9319,
#9320),(#9321,#9322),(#9323,#9324),(#9325,#9326),(#9327,#9328),(#9329,#9330),
(#9331,#9332)),.UNSPECIFIED.,.F.,.F.,.F.,(6,1,1,1,1,1,1,1,1,1,1,1,1,1,1,
1,1,1,1,1,1,1,1,1,1,1,1,1,1,1,1,1,1,1,1,1,1,1,1,1,1,1,1,1,1,1,1,1,1,1,1,
1,1,1,1,1,1,1,1,1,1,1,1,1,1,1,1,1,1,1,6),(2,2),(-1.,-0.985714285714284,
-0.97142857142857,-0.957142857142856,-0.942857142857141,-0.928571428571427,
-0.914285714285713,-0.899999999999999,-0.885714285714284,-0.87142857142857,
-0.857142857142856,-0.842857142857142,-0.828571428571428,-0.814285714285713,
-0.799999999999999,-0.785714285714285,-0.771428571428571,-0.757142857142856,
-0.742857142857142,-0.728571428571428,-0.714285714285714,-0.699999999999999,
-0.685714285714285,-0.671428571428571,-0.657142857142857,-0.642857142857142,
-0.628571428571428,-0.614285714285714,-0.6,-0.585714285714286,-0.571428571428571,
-0.557142857142857,-0.542857142857143,-0.528571428571429,-0.514285714285714,
-0.5,-0.485714285714286,-0.471428571428572,-0.457142857142857,-0.442857142857143,
-0.428571428571429,-0.414285714285714,-0.4,-0.385714285714286,-0.371428571428571,
-0.357142857142857,-0.342857142857143,-0.328571428571429,-0.314285714285714,
-0.3,-0.285714285714286,-0.271428571428571,-0.257142857142857,-0.242857142857143,
-0.228571428571429,-0.214285714285714,-0.2,-0.185714285714286,-0.171428571428571,
-0.157142857142857,-0.142857142857143,-0.128571428571429,-0.114285714285714,
-0.1,-0.0857142857142857,-0.0714285714285714,-0.0571428571428571,-0.0428571428571429,
-0.0285714285714286,-0.0142857142857143,0.),(0.,2.1),.UNSPECIFIED.);
#198=B_SPLINE_SURFACE_WITH_KNOTS('',5,1,((#9483,#9484),(#9485,#9486),(#9487,
#9488),(#9489,#9490),(#9491,#9492),(#9493,#9494),(#9495,#9496),(#9497,#9498),
(#9499,#9500),(#9501,#9502),(#9503,#9504),(#9505,#9506),(#9507,#9508),(#9509,
#9510),(#9511,#9512),(#9513,#9514),(#9515,#9516),(#9517,#9518),(#9519,#9520),
(#9521,#9522),(#9523,#9524),(#9525,#9526),(#9527,#9528),(#9529,#9530),(#9531,
#9532),(#9533,#9534),(#9535,#9536),(#9537,#9538),(#9539,#9540),(#9541,#9542),
(#9543,#9544),(#9545,#9546),(#9547,#9548),(#9549,#9550),(#9551,#9552),(#9553,
#9554),(#9555,#9556),(#9557,#9558),(#9559,#9560),(#9561,#9562),(#9563,#9564),
(#9565,#9566),(#9567,#9568),(#9569,#9570),(#9571,#9572),(#9573,#9574),(#9575,
#9576),(#9577,#9578),(#9579,#9580),(#9581,#9582),(#9583,#9584),(#9585,#9586),
(#9587,#9588),(#9589,#9590),(#9591,#9592),(#9593,#9594),(#9595,#9596),(#9597,
#9598),(#9599,#9600),(#9601,#9602),(#9603,#9604),(#9605,#9606),(#9607,#9608),
(#9609,#9610),(#9611,#9612),(#9613,#9614),(#9615,#9616),(#9617,#9618),(#9619,
#9620),(#9621,#9622),(#9623,#9624),(#9625,#9626),(#9627,#9628),(#9629,#9630),
(#9631,#9632)),.UNSPECIFIED.,.F.,.F.,.F.,(6,1,1,1,1,1,1,1,1,1,1,1,1,1,1,
1,1,1,1,1,1,1,1,1,1,1,1,1,1,1,1,1,1,1,1,1,1,1,1,1,1,1,1,1,1,1,1,1,1,1,1,
1,1,1,1,1,1,1,1,1,1,1,1,1,1,1,1,1,1,1,6),(2,2),(0.,0.0142857142857143,0.0285714285714286,
0.0428571428571429,0.0571428571428571,0.0714285714285714,0.0857142857142857,
0.1,0.114285714285714,0.128571428571429,0.142857142857143,0.157142857142857,
0.171428571428571,0.185714285714286,0.2,0.214285714285714,0.228571428571429,
0.242857142857143,0.257142857142857,0.271428571428571,0.285714285714286,
0.3,0.314285714285714,0.328571428571429,0.342857142857143,0.357142857142857,
0.371428571428571,0.385714285714286,0.4,0.414285714285714,0.428571428571429,
0.442857142857143,0.457142857142857,0.471428571428572,0.485714285714286,
0.5,0.514285714285714,0.528571428571429,0.542857142857143,0.557142857142857,
0.571428571428571,0.585714285714286,0.6,0.614285714285714,0.628571428571428,
0.642857142857142,0.657142857142857,0.671428571428571,0.685714285714285,
0.699999999999999,0.714285714285714,0.728571428571428,0.742857142857142,
0.757142857142856,0.771428571428571,0.785714285714285,0.799999999999999,
0.814285714285713,0.828571428571428,0.842857142857142,0.857142857142856,
0.87142857142857,0.885714285714284,0.899999999999999,0.914285714285713,
0.928571428571427,0.942857142857141,0.957142857142856,0.97142857142857,
0.985714285714284,1.),(0.,2.1),.UNSPECIFIED.);
#199=B_SPLINE_SURFACE_WITH_KNOTS('',5,1,((#9777,#9778),(#9779,#9780),(#9781,
#9782),(#9783,#9784),(#9785,#9786),(#9787,#9788),(#9789,#9790),(#9791,#9792),
(#9793,#9794),(#9795,#9796),(#9797,#9798),(#9799,#9800),(#9801,#9802),(#9803,
#9804),(#9805,#9806),(#9807,#9808),(#9809,#9810),(#9811,#9812),(#9813,#9814),
(#9815,#9816),(#9817,#9818),(#9819,#9820),(#9821,#9822),(#9823,#9824),(#9825,
#9826),(#9827,#9828),(#9829,#9830),(#9831,#9832),(#9833,#9834),(#9835,#9836),
(#9837,#9838),(#9839,#9840),(#9841,#9842),(#9843,#9844),(#9845,#9846),(#9847,
#9848),(#9849,#9850),(#9851,#9852),(#9853,#9854),(#9855,#9856),(#9857,#9858),
(#9859,#9860),(#9861,#9862),(#9863,#9864),(#9865,#9866),(#9867,#9868),(#9869,
#9870),(#9871,#9872),(#9873,#9874),(#9875,#9876),(#9877,#9878),(#9879,#9880),
(#9881,#9882),(#9883,#9884),(#9885,#9886),(#9887,#9888),(#9889,#9890),(#9891,
#9892),(#9893,#9894),(#9895,#9896),(#9897,#9898),(#9899,#9900),(#9901,#9902),
(#9903,#9904),(#9905,#9906),(#9907,#9908),(#9909,#9910),(#9911,#9912),(#9913,
#9914),(#9915,#9916),(#9917,#9918),(#9919,#9920),(#9921,#9922),(#9923,#9924),
(#9925,#9926)),.UNSPECIFIED.,.F.,.F.,.F.,(6,1,1,1,1,1,1,1,1,1,1,1,1,1,1,
1,1,1,1,1,1,1,1,1,1,1,1,1,1,1,1,1,1,1,1,1,1,1,1,1,1,1,1,1,1,1,1,1,1,1,1,
1,1,1,1,1,1,1,1,1,1,1,1,1,1,1,1,1,1,1,6),(2,2),(-1.,-0.985714285714284,
-0.97142857142857,-0.957142857142856,-0.942857142857141,-0.928571428571427,
-0.914285714285713,-0.899999999999999,-0.885714285714284,-0.87142857142857,
-0.857142857142856,-0.842857142857142,-0.828571428571428,-0.814285714285713,
-0.799999999999999,-0.785714285714285,-0.771428571428571,-0.757142857142856,
-0.742857142857142,-0.728571428571428,-0.714285714285714,-0.699999999999999,
-0.685714285714285,-0.671428571428571,-0.657142857142857,-0.642857142857142,
-0.628571428571428,-0.614285714285714,-0.6,-0.585714285714286,-0.571428571428571,
-0.557142857142857,-0.542857142857143,-0.528571428571429,-0.514285714285714,
-0.5,-0.485714285714286,-0.471428571428572,-0.457142857142857,-0.442857142857143,
-0.428571428571429,-0.414285714285714,-0.4,-0.385714285714286,-0.371428571428571,
-0.357142857142857,-0.342857142857143,-0.328571428571429,-0.314285714285714,
-0.3,-0.285714285714286,-0.271428571428571,-0.257142857142857,-0.242857142857143,
-0.228571428571429,-0.214285714285714,-0.2,-0.185714285714286,-0.171428571428571,
-0.157142857142857,-0.142857142857143,-0.128571428571429,-0.114285714285714,
-0.1,-0.0857142857142857,-0.0714285714285714,-0.0571428571428571,-0.0428571428571429,
-0.0285714285714286,-0.0142857142857143,0.),(0.,2.1),.UNSPECIFIED.);
#200=B_SPLINE_SURFACE_WITH_KNOTS('',5,1,((#10077,#10078),(#10079,#10080),
(#10081,#10082),(#10083,#10084),(#10085,#10086),(#10087,#10088),(#10089,
#10090),(#10091,#10092),(#10093,#10094),(#10095,#10096),(#10097,#10098),
(#10099,#10100),(#10101,#10102),(#10103,#10104),(#10105,#10106),(#10107,
#10108),(#10109,#10110),(#10111,#10112),(#10113,#10114),(#10115,#10116),
(#10117,#10118),(#10119,#10120),(#10121,#10122),(#10123,#10124),(#10125,
#10126),(#10127,#10128),(#10129,#10130),(#10131,#10132),(#10133,#10134),
(#10135,#10136),(#10137,#10138),(#10139,#10140),(#10141,#10142),(#10143,
#10144),(#10145,#10146),(#10147,#10148),(#10149,#10150),(#10151,#10152),
(#10153,#10154),(#10155,#10156),(#10157,#10158),(#10159,#10160),(#10161,
#10162),(#10163,#10164),(#10165,#10166),(#10167,#10168),(#10169,#10170),
(#10171,#10172),(#10173,#10174),(#10175,#10176),(#10177,#10178),(#10179,
#10180),(#10181,#10182),(#10183,#10184),(#10185,#10186),(#10187,#10188),
(#10189,#10190),(#10191,#10192),(#10193,#10194),(#10195,#10196),(#10197,
#10198),(#10199,#10200),(#10201,#10202),(#10203,#10204),(#10205,#10206),
(#10207,#10208),(#10209,#10210),(#10211,#10212),(#10213,#10214),(#10215,
#10216),(#10217,#10218),(#10219,#10220),(#10221,#10222),(#10223,#10224),
(#10225,#10226)),.UNSPECIFIED.,.F.,.F.,.F.,(6,1,1,1,1,1,1,1,1,1,1,1,1,1,
1,1,1,1,1,1,1,1,1,1,1,1,1,1,1,1,1,1,1,1,1,1,1,1,1,1,1,1,1,1,1,1,1,1,1,1,
1,1,1,1,1,1,1,1,1,1,1,1,1,1,1,1,1,1,1,1,6),(2,2),(0.,0.0142857142857143,
0.0285714285714286,0.0428571428571429,0.0571428571428571,0.0714285714285714,
0.0857142857142857,0.1,0.114285714285714,0.128571428571429,0.142857142857143,
0.157142857142857,0.171428571428571,0.185714285714286,0.2,0.214285714285714,
0.228571428571429,0.242857142857143,0.257142857142857,0.271428571428571,
0.285714285714286,0.3,0.314285714285714,0.328571428571429,0.342857142857143,
0.357142857142857,0.371428571428571,0.385714285714286,0.4,0.414285714285714,
0.428571428571429,0.442857142857143,0.457142857142857,0.471428571428572,
0.485714285714286,0.5,0.514285714285714,0.528571428571429,0.542857142857143,
0.557142857142857,0.571428571428571,0.585714285714286,0.6,0.614285714285714,
0.628571428571428,0.642857142857142,0.657142857142857,0.671428571428571,
0.685714285714285,0.699999999999999,0.714285714285714,0.728571428571428,
0.742857142857142,0.757142857142856,0.771428571428571,0.785714285714285,
0.799999999999999,0.814285714285713,0.828571428571428,0.842857142857142,
0.857142857142856,0.87142857142857,0.885714285714284,0.899999999999999,
0.914285714285713,0.928571428571427,0.942857142857141,0.957142857142856,
0.97142857142857,0.985714285714284,1.),(0.,2.1),.UNSPECIFIED.);
#201=B_SPLINE_SURFACE_WITH_KNOTS('',5,1,((#10371,#10372),(#10373,#10374),
(#10375,#10376),(#10377,#10378),(#10379,#10380),(#10381,#10382),(#10383,
#10384),(#10385,#10386),(#10387,#10388),(#10389,#10390),(#10391,#10392),
(#10393,#10394),(#10395,#10396),(#10397,#10398),(#10399,#10400),(#10401,
#10402),(#10403,#10404),(#10405,#10406),(#10407,#10408),(#10409,#10410),
(#10411,#10412),(#10413,#10414),(#10415,#10416),(#10417,#10418),(#10419,
#10420),(#10421,#10422),(#10423,#10424),(#10425,#10426),(#10427,#10428),
(#10429,#10430),(#10431,#10432),(#10433,#10434),(#10435,#10436),(#10437,
#10438),(#10439,#10440),(#10441,#10442),(#10443,#10444),(#10445,#10446),
(#10447,#10448),(#10449,#10450),(#10451,#10452),(#10453,#10454),(#10455,
#10456),(#10457,#10458),(#10459,#10460),(#10461,#10462),(#10463,#10464),
(#10465,#10466),(#10467,#10468),(#10469,#10470),(#10471,#10472),(#10473,
#10474),(#10475,#10476),(#10477,#10478),(#10479,#10480),(#10481,#10482),
(#10483,#10484),(#10485,#10486),(#10487,#10488),(#10489,#10490),(#10491,
#10492),(#10493,#10494),(#10495,#10496),(#10497,#10498),(#10499,#10500),
(#10501,#10502),(#10503,#10504),(#10505,#10506),(#10507,#10508),(#10509,
#10510),(#10511,#10512),(#10513,#10514),(#10515,#10516),(#10517,#10518),
(#10519,#10520)),.UNSPECIFIED.,.F.,.F.,.F.,(6,1,1,1,1,1,1,1,1,1,1,1,1,1,
1,1,1,1,1,1,1,1,1,1,1,1,1,1,1,1,1,1,1,1,1,1,1,1,1,1,1,1,1,1,1,1,1,1,1,1,
1,1,1,1,1,1,1,1,1,1,1,1,1,1,1,1,1,1,1,1,6),(2,2),(-1.,-0.985714285714284,
-0.97142857142857,-0.957142857142856,-0.942857142857141,-0.928571428571427,
-0.914285714285713,-0.899999999999999,-0.885714285714284,-0.87142857142857,
-0.857142857142856,-0.842857142857142,-0.828571428571428,-0.814285714285713,
-0.799999999999999,-0.785714285714285,-0.771428571428571,-0.757142857142856,
-0.742857142857142,-0.728571428571428,-0.714285714285714,-0.699999999999999,
-0.685714285714285,-0.671428571428571,-0.657142857142857,-0.642857142857142,
-0.628571428571428,-0.614285714285714,-0.6,-0.585714285714286,-0.571428571428571,
-0.557142857142857,-0.542857142857143,-0.528571428571429,-0.514285714285714,
-0.5,-0.485714285714286,-0.471428571428572,-0.457142857142857,-0.442857142857143,
-0.428571428571429,-0.414285714285714,-0.4,-0.385714285714286,-0.371428571428571,
-0.357142857142857,-0.342857142857143,-0.328571428571429,-0.314285714285714,
-0.3,-0.285714285714286,-0.271428571428571,-0.257142857142857,-0.242857142857143,
-0.228571428571429,-0.214285714285714,-0.2,-0.185714285714286,-0.171428571428571,
-0.157142857142857,-0.142857142857143,-0.128571428571429,-0.114285714285714,
-0.1,-0.0857142857142857,-0.0714285714285714,-0.0571428571428571,-0.0428571428571429,
-0.0285714285714286,-0.0142857142857143,0.),(0.,2.1),.UNSPECIFIED.);
#202=B_SPLINE_SURFACE_WITH_KNOTS('',5,1,((#10671,#10672),(#10673,#10674),
(#10675,#10676),(#10677,#10678),(#10679,#10680),(#10681,#10682),(#10683,
#10684),(#10685,#10686),(#10687,#10688),(#10689,#10690),(#10691,#10692),
(#10693,#10694),(#10695,#10696),(#10697,#10698),(#10699,#10700),(#10701,
#10702),(#10703,#10704),(#10705,#10706),(#10707,#10708),(#10709,#10710),
(#10711,#10712),(#10713,#10714),(#10715,#10716),(#10717,#10718),(#10719,
#10720),(#10721,#10722),(#10723,#10724),(#10725,#10726),(#10727,#10728),
(#10729,#10730),(#10731,#10732),(#10733,#10734),(#10735,#10736),(#10737,
#10738),(#10739,#10740),(#10741,#10742),(#10743,#10744),(#10745,#10746),
(#10747,#10748),(#10749,#10750),(#10751,#10752),(#10753,#10754),(#10755,
#10756),(#10757,#10758),(#10759,#10760),(#10761,#10762),(#10763,#10764),
(#10765,#10766),(#10767,#10768),(#10769,#10770),(#10771,#10772),(#10773,
#10774),(#10775,#10776),(#10777,#10778),(#10779,#10780),(#10781,#10782),
(#10783,#10784),(#10785,#10786),(#10787,#10788),(#10789,#10790),(#10791,
#10792),(#10793,#10794),(#10795,#10796),(#10797,#10798),(#10799,#10800),
(#10801,#10802),(#10803,#10804),(#10805,#10806),(#10807,#10808),(#10809,
#10810),(#10811,#10812),(#10813,#10814),(#10815,#10816),(#10817,#10818),
(#10819,#10820)),.UNSPECIFIED.,.F.,.F.,.F.,(6,1,1,1,1,1,1,1,1,1,1,1,1,1,
1,1,1,1,1,1,1,1,1,1,1,1,1,1,1,1,1,1,1,1,1,1,1,1,1,1,1,1,1,1,1,1,1,1,1,1,
1,1,1,1,1,1,1,1,1,1,1,1,1,1,1,1,1,1,1,1,6),(2,2),(0.,0.0142857142857143,
0.0285714285714286,0.0428571428571429,0.0571428571428571,0.0714285714285714,
0.0857142857142857,0.1,0.114285714285714,0.128571428571429,0.142857142857143,
0.157142857142857,0.171428571428571,0.185714285714286,0.2,0.214285714285714,
0.228571428571429,0.242857142857143,0.257142857142857,0.271428571428571,
0.285714285714286,0.3,0.314285714285714,0.328571428571429,0.342857142857143,
0.357142857142857,0.371428571428571,0.385714285714286,0.4,0.414285714285714,
0.428571428571429,0.442857142857143,0.457142857142857,0.471428571428572,
0.485714285714286,0.5,0.514285714285714,0.528571428571429,0.542857142857143,
0.557142857142857,0.571428571428571,0.585714285714286,0.6,0.614285714285714,
0.628571428571428,0.642857142857142,0.657142857142857,0.671428571428571,
0.685714285714285,0.699999999999999,0.714285714285714,0.728571428571428,
0.742857142857142,0.757142857142856,0.771428571428571,0.785714285714285,
0.799999999999999,0.814285714285713,0.828571428571428,0.842857142857142,
0.857142857142856,0.87142857142857,0.885714285714284,0.899999999999999,
0.914285714285713,0.928571428571427,0.942857142857141,0.957142857142856,
0.97142857142857,0.985714285714284,1.),(0.,2.1),.UNSPECIFIED.);
#203=B_SPLINE_SURFACE_WITH_KNOTS('',5,1,((#10965,#10966),(#10967,#10968),
(#10969,#10970),(#10971,#10972),(#10973,#10974),(#10975,#10976),(#10977,
#10978),(#10979,#10980),(#10981,#10982),(#10983,#10984),(#10985,#10986),
(#10987,#10988),(#10989,#10990),(#10991,#10992),(#10993,#10994),(#10995,
#10996),(#10997,#10998),(#10999,#11000),(#11001,#11002),(#11003,#11004),
(#11005,#11006),(#11007,#11008),(#11009,#11010),(#11011,#11012),(#11013,
#11014),(#11015,#11016),(#11017,#11018),(#11019,#11020),(#11021,#11022),
(#11023,#11024),(#11025,#11026),(#11027,#11028),(#11029,#11030),(#11031,
#11032),(#11033,#11034),(#11035,#11036),(#11037,#11038),(#11039,#11040),
(#11041,#11042),(#11043,#11044),(#11045,#11046),(#11047,#11048),(#11049,
#11050),(#11051,#11052),(#11053,#11054),(#11055,#11056),(#11057,#11058),
(#11059,#11060),(#11061,#11062),(#11063,#11064),(#11065,#11066),(#11067,
#11068),(#11069,#11070),(#11071,#11072),(#11073,#11074),(#11075,#11076),
(#11077,#11078),(#11079,#11080),(#11081,#11082),(#11083,#11084),(#11085,
#11086),(#11087,#11088),(#11089,#11090),(#11091,#11092),(#11093,#11094),
(#11095,#11096),(#11097,#11098),(#11099,#11100),(#11101,#11102),(#11103,
#11104),(#11105,#11106),(#11107,#11108),(#11109,#11110),(#11111,#11112),
(#11113,#11114)),.UNSPECIFIED.,.F.,.F.,.F.,(6,1,1,1,1,1,1,1,1,1,1,1,1,1,
1,1,1,1,1,1,1,1,1,1,1,1,1,1,1,1,1,1,1,1,1,1,1,1,1,1,1,1,1,1,1,1,1,1,1,1,
1,1,1,1,1,1,1,1,1,1,1,1,1,1,1,1,1,1,1,1,6),(2,2),(-1.,-0.985714285714284,
-0.97142857142857,-0.957142857142856,-0.942857142857141,-0.928571428571427,
-0.914285714285713,-0.899999999999999,-0.885714285714284,-0.87142857142857,
-0.857142857142856,-0.842857142857142,-0.828571428571428,-0.814285714285713,
-0.799999999999999,-0.785714285714285,-0.771428571428571,-0.757142857142856,
-0.742857142857142,-0.728571428571428,-0.714285714285714,-0.699999999999999,
-0.685714285714285,-0.671428571428571,-0.657142857142857,-0.642857142857142,
-0.628571428571428,-0.614285714285714,-0.6,-0.585714285714286,-0.571428571428571,
-0.557142857142857,-0.542857142857143,-0.528571428571429,-0.514285714285714,
-0.5,-0.485714285714286,-0.471428571428572,-0.457142857142857,-0.442857142857143,
-0.428571428571429,-0.414285714285714,-0.4,-0.385714285714286,-0.371428571428571,
-0.357142857142857,-0.342857142857143,-0.328571428571429,-0.314285714285714,
-0.3,-0.285714285714286,-0.271428571428571,-0.257142857142857,-0.242857142857143,
-0.228571428571429,-0.214285714285714,-0.2,-0.185714285714286,-0.171428571428571,
-0.157142857142857,-0.142857142857143,-0.128571428571429,-0.114285714285714,
-0.1,-0.0857142857142857,-0.0714285714285714,-0.0571428571428571,-0.0428571428571429,
-0.0285714285714286,-0.0142857142857143,0.),(0.,2.1),.UNSPECIFIED.);
#204=B_SPLINE_SURFACE_WITH_KNOTS('',5,1,((#11265,#11266),(#11267,#11268),
(#11269,#11270),(#11271,#11272),(#11273,#11274),(#11275,#11276),(#11277,
#11278),(#11279,#11280),(#11281,#11282),(#11283,#11284),(#11285,#11286),
(#11287,#11288),(#11289,#11290),(#11291,#11292),(#11293,#11294),(#11295,
#11296),(#11297,#11298),(#11299,#11300),(#11301,#11302),(#11303,#11304),
(#11305,#11306),(#11307,#11308),(#11309,#11310),(#11311,#11312),(#11313,
#11314),(#11315,#11316),(#11317,#11318),(#11319,#11320),(#11321,#11322),
(#11323,#11324),(#11325,#11326),(#11327,#11328),(#11329,#11330),(#11331,
#11332),(#11333,#11334),(#11335,#11336),(#11337,#11338),(#11339,#11340),
(#11341,#11342),(#11343,#11344),(#11345,#11346),(#11347,#11348),(#11349,
#11350),(#11351,#11352),(#11353,#11354),(#11355,#11356),(#11357,#11358),
(#11359,#11360),(#11361,#11362),(#11363,#11364),(#11365,#11366),(#11367,
#11368),(#11369,#11370),(#11371,#11372),(#11373,#11374),(#11375,#11376),
(#11377,#11378),(#11379,#11380),(#11381,#11382),(#11383,#11384),(#11385,
#11386),(#11387,#11388),(#11389,#11390),(#11391,#11392),(#11393,#11394),
(#11395,#11396),(#11397,#11398),(#11399,#11400),(#11401,#11402),(#11403,
#11404),(#11405,#11406),(#11407,#11408),(#11409,#11410),(#11411,#11412),
(#11413,#11414)),.UNSPECIFIED.,.F.,.F.,.F.,(6,1,1,1,1,1,1,1,1,1,1,1,1,1,
1,1,1,1,1,1,1,1,1,1,1,1,1,1,1,1,1,1,1,1,1,1,1,1,1,1,1,1,1,1,1,1,1,1,1,1,
1,1,1,1,1,1,1,1,1,1,1,1,1,1,1,1,1,1,1,1,6),(2,2),(0.,0.0142857142857143,
0.0285714285714286,0.0428571428571429,0.0571428571428571,0.0714285714285714,
0.0857142857142857,0.1,0.114285714285714,0.128571428571429,0.142857142857143,
0.157142857142857,0.171428571428571,0.185714285714286,0.2,0.214285714285714,
0.228571428571429,0.242857142857143,0.257142857142857,0.271428571428571,
0.285714285714286,0.3,0.314285714285714,0.328571428571429,0.342857142857143,
0.357142857142857,0.371428571428571,0.385714285714286,0.4,0.414285714285714,
0.428571428571429,0.442857142857143,0.457142857142857,0.471428571428572,
0.485714285714286,0.5,0.514285714285714,0.528571428571429,0.542857142857143,
0.557142857142857,0.571428571428571,0.585714285714286,0.6,0.614285714285714,
0.628571428571428,0.642857142857142,0.657142857142857,0.671428571428571,
0.685714285714285,0.699999999999999,0.714285714285714,0.728571428571428,
0.742857142857142,0.757142857142856,0.771428571428571,0.785714285714285,
0.799999999999999,0.814285714285713,0.828571428571428,0.842857142857142,
0.857142857142856,0.87142857142857,0.885714285714284,0.899999999999999,
0.914285714285713,0.928571428571427,0.942857142857141,0.957142857142856,
0.97142857142857,0.985714285714284,1.),(0.,2.1),.UNSPECIFIED.);
#205=B_SPLINE_SURFACE_WITH_KNOTS('',5,1,((#11559,#11560),(#11561,#11562),
(#11563,#11564),(#11565,#11566),(#11567,#11568),(#11569,#11570),(#11571,
#11572),(#11573,#11574),(#11575,#11576),(#11577,#11578),(#11579,#11580),
(#11581,#11582),(#11583,#11584),(#11585,#11586),(#11587,#11588),(#11589,
#11590),(#11591,#11592),(#11593,#11594),(#11595,#11596),(#11597,#11598),
(#11599,#11600),(#11601,#11602),(#11603,#11604),(#11605,#11606),(#11607,
#11608),(#11609,#11610),(#11611,#11612),(#11613,#11614),(#11615,#11616),
(#11617,#11618),(#11619,#11620),(#11621,#11622),(#11623,#11624),(#11625,
#11626),(#11627,#11628),(#11629,#11630),(#11631,#11632),(#11633,#11634),
(#11635,#11636),(#11637,#11638),(#11639,#11640),(#11641,#11642),(#11643,
#11644),(#11645,#11646),(#11647,#11648),(#11649,#11650),(#11651,#11652),
(#11653,#11654),(#11655,#11656),(#11657,#11658),(#11659,#11660),(#11661,
#11662),(#11663,#11664),(#11665,#11666),(#11667,#11668),(#11669,#11670),
(#11671,#11672),(#11673,#11674),(#11675,#11676),(#11677,#11678),(#11679,
#11680),(#11681,#11682),(#11683,#11684),(#11685,#11686),(#11687,#11688),
(#11689,#11690),(#11691,#11692),(#11693,#11694),(#11695,#11696),(#11697,
#11698),(#11699,#11700),(#11701,#11702),(#11703,#11704),(#11705,#11706),
(#11707,#11708)),.UNSPECIFIED.,.F.,.F.,.F.,(6,1,1,1,1,1,1,1,1,1,1,1,1,1,
1,1,1,1,1,1,1,1,1,1,1,1,1,1,1,1,1,1,1,1,1,1,1,1,1,1,1,1,1,1,1,1,1,1,1,1,
1,1,1,1,1,1,1,1,1,1,1,1,1,1,1,1,1,1,1,1,6),(2,2),(-1.,-0.985714285714284,
-0.97142857142857,-0.957142857142856,-0.942857142857141,-0.928571428571427,
-0.914285714285713,-0.899999999999999,-0.885714285714284,-0.87142857142857,
-0.857142857142856,-0.842857142857142,-0.828571428571428,-0.814285714285713,
-0.799999999999999,-0.785714285714285,-0.771428571428571,-0.757142857142856,
-0.742857142857142,-0.728571428571428,-0.714285714285714,-0.699999999999999,
-0.685714285714285,-0.671428571428571,-0.657142857142857,-0.642857142857142,
-0.628571428571428,-0.614285714285714,-0.6,-0.585714285714286,-0.571428571428571,
-0.557142857142857,-0.542857142857143,-0.528571428571429,-0.514285714285714,
-0.5,-0.485714285714286,-0.471428571428572,-0.457142857142857,-0.442857142857143,
-0.428571428571429,-0.414285714285714,-0.4,-0.385714285714286,-0.371428571428571,
-0.357142857142857,-0.342857142857143,-0.328571428571429,-0.314285714285714,
-0.3,-0.285714285714286,-0.271428571428571,-0.257142857142857,-0.242857142857143,
-0.228571428571429,-0.214285714285714,-0.2,-0.185714285714286,-0.171428571428571,
-0.157142857142857,-0.142857142857143,-0.128571428571429,-0.114285714285714,
-0.1,-0.0857142857142857,-0.0714285714285714,-0.0571428571428571,-0.0428571428571429,
-0.0285714285714286,-0.0142857142857143,0.),(0.,2.1),.UNSPECIFIED.);
#206=B_SPLINE_SURFACE_WITH_KNOTS('',5,1,((#11859,#11860),(#11861,#11862),
(#11863,#11864),(#11865,#11866),(#11867,#11868),(#11869,#11870),(#11871,
#11872),(#11873,#11874),(#11875,#11876),(#11877,#11878),(#11879,#11880),
(#11881,#11882),(#11883,#11884),(#11885,#11886),(#11887,#11888),(#11889,
#11890),(#11891,#11892),(#11893,#11894),(#11895,#11896),(#11897,#11898),
(#11899,#11900),(#11901,#11902),(#11903,#11904),(#11905,#11906),(#11907,
#11908),(#11909,#11910),(#11911,#11912),(#11913,#11914),(#11915,#11916),
(#11917,#11918),(#11919,#11920),(#11921,#11922),(#11923,#11924),(#11925,
#11926),(#11927,#11928),(#11929,#11930),(#11931,#11932),(#11933,#11934),
(#11935,#11936),(#11937,#11938),(#11939,#11940),(#11941,#11942),(#11943,
#11944),(#11945,#11946),(#11947,#11948),(#11949,#11950),(#11951,#11952),
(#11953,#11954),(#11955,#11956),(#11957,#11958),(#11959,#11960),(#11961,
#11962),(#11963,#11964),(#11965,#11966),(#11967,#11968),(#11969,#11970),
(#11971,#11972),(#11973,#11974),(#11975,#11976),(#11977,#11978),(#11979,
#11980),(#11981,#11982),(#11983,#11984),(#11985,#11986),(#11987,#11988),
(#11989,#11990),(#11991,#11992),(#11993,#11994),(#11995,#11996),(#11997,
#11998),(#11999,#12000),(#12001,#12002),(#12003,#12004),(#12005,#12006),
(#12007,#12008)),.UNSPECIFIED.,.F.,.F.,.F.,(6,1,1,1,1,1,1,1,1,1,1,1,1,1,
1,1,1,1,1,1,1,1,1,1,1,1,1,1,1,1,1,1,1,1,1,1,1,1,1,1,1,1,1,1,1,1,1,1,1,1,
1,1,1,1,1,1,1,1,1,1,1,1,1,1,1,1,1,1,1,1,6),(2,2),(0.,0.0142857142857143,
0.0285714285714286,0.0428571428571429,0.0571428571428571,0.0714285714285714,
0.0857142857142857,0.1,0.114285714285714,0.128571428571429,0.142857142857143,
0.157142857142857,0.171428571428571,0.185714285714286,0.2,0.214285714285714,
0.228571428571429,0.242857142857143,0.257142857142857,0.271428571428571,
0.285714285714286,0.3,0.314285714285714,0.328571428571429,0.342857142857143,
0.357142857142857,0.371428571428571,0.385714285714286,0.4,0.414285714285714,
0.428571428571429,0.442857142857143,0.457142857142857,0.471428571428572,
0.485714285714286,0.5,0.514285714285714,0.528571428571429,0.542857142857143,
0.557142857142857,0.571428571428571,0.585714285714286,0.6,0.614285714285714,
0.628571428571428,0.642857142857142,0.657142857142857,0.671428571428571,
0.685714285714285,0.699999999999999,0.714285714285714,0.728571428571428,
0.742857142857142,0.757142857142856,0.771428571428571,0.785714285714285,
0.799999999999999,0.814285714285713,0.828571428571428,0.842857142857142,
0.857142857142856,0.87142857142857,0.885714285714284,0.899999999999999,
0.914285714285713,0.928571428571427,0.942857142857141,0.957142857142856,
0.97142857142857,0.985714285714284,1.),(0.,2.1),.UNSPECIFIED.);
#207=B_SPLINE_SURFACE_WITH_KNOTS('',5,1,((#12153,#12154),(#12155,#12156),
(#12157,#12158),(#12159,#12160),(#12161,#12162),(#12163,#12164),(#12165,
#12166),(#12167,#12168),(#12169,#12170),(#12171,#12172),(#12173,#12174),
(#12175,#12176),(#12177,#12178),(#12179,#12180),(#12181,#12182),(#12183,
#12184),(#12185,#12186),(#12187,#12188),(#12189,#12190),(#12191,#12192),
(#12193,#12194),(#12195,#12196),(#12197,#12198),(#12199,#12200),(#12201,
#12202),(#12203,#12204),(#12205,#12206),(#12207,#12208),(#12209,#12210),
(#12211,#12212),(#12213,#12214),(#12215,#12216),(#12217,#12218),(#12219,
#12220),(#12221,#12222),(#12223,#12224),(#12225,#12226),(#12227,#12228),
(#12229,#12230),(#12231,#12232),(#12233,#12234),(#12235,#12236),(#12237,
#12238),(#12239,#12240),(#12241,#12242),(#12243,#12244),(#12245,#12246),
(#12247,#12248),(#12249,#12250),(#12251,#12252),(#12253,#12254),(#12255,
#12256),(#12257,#12258),(#12259,#12260),(#12261,#12262),(#12263,#12264),
(#12265,#12266),(#12267,#12268),(#12269,#12270),(#12271,#12272),(#12273,
#12274),(#12275,#12276),(#12277,#12278),(#12279,#12280),(#12281,#12282),
(#12283,#12284),(#12285,#12286),(#12287,#12288),(#12289,#12290),(#12291,
#12292),(#12293,#12294),(#12295,#12296),(#12297,#12298),(#12299,#12300),
(#12301,#12302)),.UNSPECIFIED.,.F.,.F.,.F.,(6,1,1,1,1,1,1,1,1,1,1,1,1,1,
1,1,1,1,1,1,1,1,1,1,1,1,1,1,1,1,1,1,1,1,1,1,1,1,1,1,1,1,1,1,1,1,1,1,1,1,
1,1,1,1,1,1,1,1,1,1,1,1,1,1,1,1,1,1,1,1,6),(2,2),(-1.,-0.985714285714284,
-0.97142857142857,-0.957142857142856,-0.942857142857141,-0.928571428571427,
-0.914285714285713,-0.899999999999999,-0.885714285714284,-0.87142857142857,
-0.857142857142856,-0.842857142857142,-0.828571428571428,-0.814285714285713,
-0.799999999999999,-0.785714285714285,-0.771428571428571,-0.757142857142856,
-0.742857142857142,-0.728571428571428,-0.714285714285714,-0.699999999999999,
-0.685714285714285,-0.671428571428571,-0.657142857142857,-0.642857142857142,
-0.628571428571428,-0.614285714285714,-0.6,-0.585714285714286,-0.571428571428571,
-0.557142857142857,-0.542857142857143,-0.528571428571429,-0.514285714285714,
-0.5,-0.485714285714286,-0.471428571428572,-0.457142857142857,-0.442857142857143,
-0.428571428571429,-0.414285714285714,-0.4,-0.385714285714286,-0.371428571428571,
-0.357142857142857,-0.342857142857143,-0.328571428571429,-0.314285714285714,
-0.3,-0.285714285714286,-0.271428571428571,-0.257142857142857,-0.242857142857143,
-0.228571428571429,-0.214285714285714,-0.2,-0.185714285714286,-0.171428571428571,
-0.157142857142857,-0.142857142857143,-0.128571428571429,-0.114285714285714,
-0.1,-0.0857142857142857,-0.0714285714285714,-0.0571428571428571,-0.0428571428571429,
-0.0285714285714286,-0.0142857142857143,0.),(0.,2.1),.UNSPECIFIED.);
#208=B_SPLINE_SURFACE_WITH_KNOTS('',5,1,((#12453,#12454),(#12455,#12456),
(#12457,#12458),(#12459,#12460),(#12461,#12462),(#12463,#12464),(#12465,
#12466),(#12467,#12468),(#12469,#12470),(#12471,#12472),(#12473,#12474),
(#12475,#12476),(#12477,#12478),(#12479,#12480),(#12481,#12482),(#12483,
#12484),(#12485,#12486),(#12487,#12488),(#12489,#12490),(#12491,#12492),
(#12493,#12494),(#12495,#12496),(#12497,#12498),(#12499,#12500),(#12501,
#12502),(#12503,#12504),(#12505,#12506),(#12507,#12508),(#12509,#12510),
(#12511,#12512),(#12513,#12514),(#12515,#12516),(#12517,#12518),(#12519,
#12520),(#12521,#12522),(#12523,#12524),(#12525,#12526),(#12527,#12528),
(#12529,#12530),(#12531,#12532),(#12533,#12534),(#12535,#12536),(#12537,
#12538),(#12539,#12540),(#12541,#12542),(#12543,#12544),(#12545,#12546),
(#12547,#12548),(#12549,#12550),(#12551,#12552),(#12553,#12554),(#12555,
#12556),(#12557,#12558),(#12559,#12560),(#12561,#12562),(#12563,#12564),
(#12565,#12566),(#12567,#12568),(#12569,#12570),(#12571,#12572),(#12573,
#12574),(#12575,#12576),(#12577,#12578),(#12579,#12580),(#12581,#12582),
(#12583,#12584),(#12585,#12586),(#12587,#12588),(#12589,#12590),(#12591,
#12592),(#12593,#12594),(#12595,#12596),(#12597,#12598),(#12599,#12600),
(#12601,#12602)),.UNSPECIFIED.,.F.,.F.,.F.,(6,1,1,1,1,1,1,1,1,1,1,1,1,1,
1,1,1,1,1,1,1,1,1,1,1,1,1,1,1,1,1,1,1,1,1,1,1,1,1,1,1,1,1,1,1,1,1,1,1,1,
1,1,1,1,1,1,1,1,1,1,1,1,1,1,1,1,1,1,1,1,6),(2,2),(0.,0.0142857142857143,
0.0285714285714286,0.0428571428571429,0.0571428571428571,0.0714285714285714,
0.0857142857142857,0.1,0.114285714285714,0.128571428571429,0.142857142857143,
0.157142857142857,0.171428571428571,0.185714285714286,0.2,0.214285714285714,
0.228571428571429,0.242857142857143,0.257142857142857,0.271428571428571,
0.285714285714286,0.3,0.314285714285714,0.328571428571429,0.342857142857143,
0.357142857142857,0.371428571428571,0.385714285714286,0.4,0.414285714285714,
0.428571428571429,0.442857142857143,0.457142857142857,0.471428571428572,
0.485714285714286,0.5,0.514285714285714,0.528571428571429,0.542857142857143,
0.557142857142857,0.571428571428571,0.585714285714286,0.6,0.614285714285714,
0.628571428571428,0.642857142857142,0.657142857142857,0.671428571428571,
0.685714285714285,0.699999999999999,0.714285714285714,0.728571428571428,
0.742857142857142,0.757142857142856,0.771428571428571,0.785714285714285,
0.799999999999999,0.814285714285713,0.828571428571428,0.842857142857142,
0.857142857142856,0.87142857142857,0.885714285714284,0.899999999999999,
0.914285714285713,0.928571428571427,0.942857142857141,0.957142857142856,
0.97142857142857,0.985714285714284,1.),(0.,2.1),.UNSPECIFIED.);
#209=B_SPLINE_SURFACE_WITH_KNOTS('',5,1,((#12747,#12748),(#12749,#12750),
(#12751,#12752),(#12753,#12754),(#12755,#12756),(#12757,#12758),(#12759,
#12760),(#12761,#12762),(#12763,#12764),(#12765,#12766),(#12767,#12768),
(#12769,#12770),(#12771,#12772),(#12773,#12774),(#12775,#12776),(#12777,
#12778),(#12779,#12780),(#12781,#12782),(#12783,#12784),(#12785,#12786),
(#12787,#12788),(#12789,#12790),(#12791,#12792),(#12793,#12794),(#12795,
#12796),(#12797,#12798),(#12799,#12800),(#12801,#12802),(#12803,#12804),
(#12805,#12806),(#12807,#12808),(#12809,#12810),(#12811,#12812),(#12813,
#12814),(#12815,#12816),(#12817,#12818),(#12819,#12820),(#12821,#12822),
(#12823,#12824),(#12825,#12826),(#12827,#12828),(#12829,#12830),(#12831,
#12832),(#12833,#12834),(#12835,#12836),(#12837,#12838),(#12839,#12840),
(#12841,#12842),(#12843,#12844),(#12845,#12846),(#12847,#12848),(#12849,
#12850),(#12851,#12852),(#12853,#12854),(#12855,#12856),(#12857,#12858),
(#12859,#12860),(#12861,#12862),(#12863,#12864),(#12865,#12866),(#12867,
#12868),(#12869,#12870),(#12871,#12872),(#12873,#12874),(#12875,#12876),
(#12877,#12878),(#12879,#12880),(#12881,#12882),(#12883,#12884),(#12885,
#12886),(#12887,#12888),(#12889,#12890),(#12891,#12892),(#12893,#12894),
(#12895,#12896)),.UNSPECIFIED.,.F.,.F.,.F.,(6,1,1,1,1,1,1,1,1,1,1,1,1,1,
1,1,1,1,1,1,1,1,1,1,1,1,1,1,1,1,1,1,1,1,1,1,1,1,1,1,1,1,1,1,1,1,1,1,1,1,
1,1,1,1,1,1,1,1,1,1,1,1,1,1,1,1,1,1,1,1,6),(2,2),(-1.,-0.985714285714284,
-0.97142857142857,-0.957142857142856,-0.942857142857141,-0.928571428571427,
-0.914285714285713,-0.899999999999999,-0.885714285714284,-0.87142857142857,
-0.857142857142856,-0.842857142857142,-0.828571428571428,-0.814285714285713,
-0.799999999999999,-0.785714285714285,-0.771428571428571,-0.757142857142856,
-0.742857142857142,-0.728571428571428,-0.714285714285714,-0.699999999999999,
-0.685714285714285,-0.671428571428571,-0.657142857142857,-0.642857142857142,
-0.628571428571428,-0.614285714285714,-0.6,-0.585714285714286,-0.571428571428571,
-0.557142857142857,-0.542857142857143,-0.528571428571429,-0.514285714285714,
-0.5,-0.485714285714286,-0.471428571428572,-0.457142857142857,-0.442857142857143,
-0.428571428571429,-0.414285714285714,-0.4,-0.385714285714286,-0.371428571428571,
-0.357142857142857,-0.342857142857143,-0.328571428571429,-0.314285714285714,
-0.3,-0.285714285714286,-0.271428571428571,-0.257142857142857,-0.242857142857143,
-0.228571428571429,-0.214285714285714,-0.2,-0.185714285714286,-0.171428571428571,
-0.157142857142857,-0.142857142857143,-0.128571428571429,-0.114285714285714,
-0.1,-0.0857142857142857,-0.0714285714285714,-0.0571428571428571,-0.0428571428571429,
-0.0285714285714286,-0.0142857142857143,0.),(0.,2.1),.UNSPECIFIED.);
#210=B_SPLINE_SURFACE_WITH_KNOTS('',5,1,((#13047,#13048),(#13049,#13050),
(#13051,#13052),(#13053,#13054),(#13055,#13056),(#13057,#13058),(#13059,
#13060),(#13061,#13062),(#13063,#13064),(#13065,#13066),(#13067,#13068),
(#13069,#13070),(#13071,#13072),(#13073,#13074),(#13075,#13076),(#13077,
#13078),(#13079,#13080),(#13081,#13082),(#13083,#13084),(#13085,#13086),
(#13087,#13088),(#13089,#13090),(#13091,#13092),(#13093,#13094),(#13095,
#13096),(#13097,#13098),(#13099,#13100),(#13101,#13102),(#13103,#13104),
(#13105,#13106),(#13107,#13108),(#13109,#13110),(#13111,#13112),(#13113,
#13114),(#13115,#13116),(#13117,#13118),(#13119,#13120),(#13121,#13122),
(#13123,#13124),(#13125,#13126),(#13127,#13128),(#13129,#13130),(#13131,
#13132),(#13133,#13134),(#13135,#13136),(#13137,#13138),(#13139,#13140),
(#13141,#13142),(#13143,#13144),(#13145,#13146),(#13147,#13148),(#13149,
#13150),(#13151,#13152),(#13153,#13154),(#13155,#13156),(#13157,#13158),
(#13159,#13160),(#13161,#13162),(#13163,#13164),(#13165,#13166),(#13167,
#13168),(#13169,#13170),(#13171,#13172),(#13173,#13174),(#13175,#13176),
(#13177,#13178),(#13179,#13180),(#13181,#13182),(#13183,#13184),(#13185,
#13186),(#13187,#13188),(#13189,#13190),(#13191,#13192),(#13193,#13194),
(#13195,#13196)),.UNSPECIFIED.,.F.,.F.,.F.,(6,1,1,1,1,1,1,1,1,1,1,1,1,1,
1,1,1,1,1,1,1,1,1,1,1,1,1,1,1,1,1,1,1,1,1,1,1,1,1,1,1,1,1,1,1,1,1,1,1,1,
1,1,1,1,1,1,1,1,1,1,1,1,1,1,1,1,1,1,1,1,6),(2,2),(0.,0.0142857142857143,
0.0285714285714286,0.0428571428571429,0.0571428571428571,0.0714285714285714,
0.0857142857142857,0.1,0.114285714285714,0.128571428571429,0.142857142857143,
0.157142857142857,0.171428571428571,0.185714285714286,0.2,0.214285714285714,
0.228571428571429,0.242857142857143,0.257142857142857,0.271428571428571,
0.285714285714286,0.3,0.314285714285714,0.328571428571429,0.342857142857143,
0.357142857142857,0.371428571428571,0.385714285714286,0.4,0.414285714285714,
0.428571428571429,0.442857142857143,0.457142857142857,0.471428571428572,
0.485714285714286,0.5,0.514285714285714,0.528571428571429,0.542857142857143,
0.557142857142857,0.571428571428571,0.585714285714286,0.6,0.614285714285714,
0.628571428571428,0.642857142857142,0.657142857142857,0.671428571428571,
0.685714285714285,0.699999999999999,0.714285714285714,0.728571428571428,
0.742857142857142,0.757142857142856,0.771428571428571,0.785714285714285,
0.799999999999999,0.814285714285713,0.828571428571428,0.842857142857142,
0.857142857142856,0.87142857142857,0.885714285714284,0.899999999999999,
0.914285714285713,0.928571428571427,0.942857142857141,0.957142857142856,
0.97142857142857,0.985714285714284,1.),(0.,2.1),.UNSPECIFIED.);
#211=B_SPLINE_SURFACE_WITH_KNOTS('',5,1,((#13341,#13342),(#13343,#13344),
(#13345,#13346),(#13347,#13348),(#13349,#13350),(#13351,#13352),(#13353,
#13354),(#13355,#13356),(#13357,#13358),(#13359,#13360),(#13361,#13362),
(#13363,#13364),(#13365,#13366),(#13367,#13368),(#13369,#13370),(#13371,
#13372),(#13373,#13374),(#13375,#13376),(#13377,#13378),(#13379,#13380),
(#13381,#13382),(#13383,#13384),(#13385,#13386),(#13387,#13388),(#13389,
#13390),(#13391,#13392),(#13393,#13394),(#13395,#13396),(#13397,#13398),
(#13399,#13400),(#13401,#13402),(#13403,#13404),(#13405,#13406),(#13407,
#13408),(#13409,#13410),(#13411,#13412),(#13413,#13414),(#13415,#13416),
(#13417,#13418),(#13419,#13420),(#13421,#13422),(#13423,#13424),(#13425,
#13426),(#13427,#13428),(#13429,#13430),(#13431,#13432),(#13433,#13434),
(#13435,#13436),(#13437,#13438),(#13439,#13440),(#13441,#13442),(#13443,
#13444),(#13445,#13446),(#13447,#13448),(#13449,#13450),(#13451,#13452),
(#13453,#13454),(#13455,#13456),(#13457,#13458),(#13459,#13460),(#13461,
#13462),(#13463,#13464),(#13465,#13466),(#13467,#13468),(#13469,#13470),
(#13471,#13472),(#13473,#13474),(#13475,#13476),(#13477,#13478),(#13479,
#13480),(#13481,#13482),(#13483,#13484),(#13485,#13486),(#13487,#13488),
(#13489,#13490)),.UNSPECIFIED.,.F.,.F.,.F.,(6,1,1,1,1,1,1,1,1,1,1,1,1,1,
1,1,1,1,1,1,1,1,1,1,1,1,1,1,1,1,1,1,1,1,1,1,1,1,1,1,1,1,1,1,1,1,1,1,1,1,
1,1,1,1,1,1,1,1,1,1,1,1,1,1,1,1,1,1,1,1,6),(2,2),(-1.,-0.985714285714284,
-0.97142857142857,-0.957142857142856,-0.942857142857141,-0.928571428571427,
-0.914285714285713,-0.899999999999999,-0.885714285714284,-0.87142857142857,
-0.857142857142856,-0.842857142857142,-0.828571428571428,-0.814285714285713,
-0.799999999999999,-0.785714285714285,-0.771428571428571,-0.757142857142856,
-0.742857142857142,-0.728571428571428,-0.714285714285714,-0.699999999999999,
-0.685714285714285,-0.671428571428571,-0.657142857142857,-0.642857142857142,
-0.628571428571428,-0.614285714285714,-0.6,-0.585714285714286,-0.571428571428571,
-0.557142857142857,-0.542857142857143,-0.528571428571429,-0.514285714285714,
-0.5,-0.485714285714286,-0.471428571428572,-0.457142857142857,-0.442857142857143,
-0.428571428571429,-0.414285714285714,-0.4,-0.385714285714286,-0.371428571428571,
-0.357142857142857,-0.342857142857143,-0.328571428571429,-0.314285714285714,
-0.3,-0.285714285714286,-0.271428571428571,-0.257142857142857,-0.242857142857143,
-0.228571428571429,-0.214285714285714,-0.2,-0.185714285714286,-0.171428571428571,
-0.157142857142857,-0.142857142857143,-0.128571428571429,-0.114285714285714,
-0.1,-0.0857142857142857,-0.0714285714285714,-0.0571428571428571,-0.0428571428571429,
-0.0285714285714286,-0.0142857142857143,0.),(0.,2.1),.UNSPECIFIED.);
#212=B_SPLINE_SURFACE_WITH_KNOTS('',5,1,((#13641,#13642),(#13643,#13644),
(#13645,#13646),(#13647,#13648),(#13649,#13650),(#13651,#13652),(#13653,
#13654),(#13655,#13656),(#13657,#13658),(#13659,#13660),(#13661,#13662),
(#13663,#13664),(#13665,#13666),(#13667,#13668),(#13669,#13670),(#13671,
#13672),(#13673,#13674),(#13675,#13676),(#13677,#13678),(#13679,#13680),
(#13681,#13682),(#13683,#13684),(#13685,#13686),(#13687,#13688),(#13689,
#13690),(#13691,#13692),(#13693,#13694),(#13695,#13696),(#13697,#13698),
(#13699,#13700),(#13701,#13702),(#13703,#13704),(#13705,#13706),(#13707,
#13708),(#13709,#13710),(#13711,#13712),(#13713,#13714),(#13715,#13716),
(#13717,#13718),(#13719,#13720),(#13721,#13722),(#13723,#13724),(#13725,
#13726),(#13727,#13728),(#13729,#13730),(#13731,#13732),(#13733,#13734),
(#13735,#13736),(#13737,#13738),(#13739,#13740),(#13741,#13742),(#13743,
#13744),(#13745,#13746),(#13747,#13748),(#13749,#13750),(#13751,#13752),
(#13753,#13754),(#13755,#13756),(#13757,#13758),(#13759,#13760),(#13761,
#13762),(#13763,#13764),(#13765,#13766),(#13767,#13768),(#13769,#13770),
(#13771,#13772),(#13773,#13774),(#13775,#13776),(#13777,#13778),(#13779,
#13780),(#13781,#13782),(#13783,#13784),(#13785,#13786),(#13787,#13788),
(#13789,#13790)),.UNSPECIFIED.,.F.,.F.,.F.,(6,1,1,1,1,1,1,1,1,1,1,1,1,1,
1,1,1,1,1,1,1,1,1,1,1,1,1,1,1,1,1,1,1,1,1,1,1,1,1,1,1,1,1,1,1,1,1,1,1,1,
1,1,1,1,1,1,1,1,1,1,1,1,1,1,1,1,1,1,1,1,6),(2,2),(0.,0.0142857142857143,
0.0285714285714286,0.0428571428571429,0.0571428571428571,0.0714285714285714,
0.0857142857142857,0.1,0.114285714285714,0.128571428571429,0.142857142857143,
0.157142857142857,0.171428571428571,0.185714285714286,0.2,0.214285714285714,
0.228571428571429,0.242857142857143,0.257142857142857,0.271428571428571,
0.285714285714286,0.3,0.314285714285714,0.328571428571429,0.342857142857143,
0.357142857142857,0.371428571428571,0.385714285714286,0.4,0.414285714285714,
0.428571428571429,0.442857142857143,0.457142857142857,0.471428571428572,
0.485714285714286,0.5,0.514285714285714,0.528571428571429,0.542857142857143,
0.557142857142857,0.571428571428571,0.585714285714286,0.6,0.614285714285714,
0.628571428571428,0.642857142857142,0.657142857142857,0.671428571428571,
0.685714285714285,0.699999999999999,0.714285714285714,0.728571428571428,
0.742857142857142,0.757142857142856,0.771428571428571,0.785714285714285,
0.799999999999999,0.814285714285713,0.828571428571428,0.842857142857142,
0.857142857142856,0.87142857142857,0.885714285714284,0.899999999999999,
0.914285714285713,0.928571428571427,0.942857142857141,0.957142857142856,
0.97142857142857,0.985714285714284,1.),(0.,2.1),.UNSPECIFIED.);
#213=B_SPLINE_SURFACE_WITH_KNOTS('',5,1,((#13935,#13936),(#13937,#13938),
(#13939,#13940),(#13941,#13942),(#13943,#13944),(#13945,#13946),(#13947,
#13948),(#13949,#13950),(#13951,#13952),(#13953,#13954),(#13955,#13956),
(#13957,#13958),(#13959,#13960),(#13961,#13962),(#13963,#13964),(#13965,
#13966),(#13967,#13968),(#13969,#13970),(#13971,#13972),(#13973,#13974),
(#13975,#13976),(#13977,#13978),(#13979,#13980),(#13981,#13982),(#13983,
#13984),(#13985,#13986),(#13987,#13988),(#13989,#13990),(#13991,#13992),
(#13993,#13994),(#13995,#13996),(#13997,#13998),(#13999,#14000),(#14001,
#14002),(#14003,#14004),(#14005,#14006),(#14007,#14008),(#14009,#14010),
(#14011,#14012),(#14013,#14014),(#14015,#14016),(#14017,#14018),(#14019,
#14020),(#14021,#14022),(#14023,#14024),(#14025,#14026),(#14027,#14028),
(#14029,#14030),(#14031,#14032),(#14033,#14034),(#14035,#14036),(#14037,
#14038),(#14039,#14040),(#14041,#14042),(#14043,#14044),(#14045,#14046),
(#14047,#14048),(#14049,#14050),(#14051,#14052),(#14053,#14054),(#14055,
#14056),(#14057,#14058),(#14059,#14060),(#14061,#14062),(#14063,#14064),
(#14065,#14066),(#14067,#14068),(#14069,#14070),(#14071,#14072),(#14073,
#14074),(#14075,#14076),(#14077,#14078),(#14079,#14080),(#14081,#14082),
(#14083,#14084)),.UNSPECIFIED.,.F.,.F.,.F.,(6,1,1,1,1,1,1,1,1,1,1,1,1,1,
1,1,1,1,1,1,1,1,1,1,1,1,1,1,1,1,1,1,1,1,1,1,1,1,1,1,1,1,1,1,1,1,1,1,1,1,
1,1,1,1,1,1,1,1,1,1,1,1,1,1,1,1,1,1,1,1,6),(2,2),(-1.,-0.985714285714284,
-0.97142857142857,-0.957142857142856,-0.942857142857141,-0.928571428571427,
-0.914285714285713,-0.899999999999999,-0.885714285714284,-0.87142857142857,
-0.857142857142856,-0.842857142857142,-0.828571428571428,-0.814285714285713,
-0.799999999999999,-0.785714285714285,-0.771428571428571,-0.757142857142856,
-0.742857142857142,-0.728571428571428,-0.714285714285714,-0.699999999999999,
-0.685714285714285,-0.671428571428571,-0.657142857142857,-0.642857142857142,
-0.628571428571428,-0.614285714285714,-0.6,-0.585714285714286,-0.571428571428571,
-0.557142857142857,-0.542857142857143,-0.528571428571429,-0.514285714285714,
-0.5,-0.485714285714286,-0.471428571428572,-0.457142857142857,-0.442857142857143,
-0.428571428571429,-0.414285714285714,-0.4,-0.385714285714286,-0.371428571428571,
-0.357142857142857,-0.342857142857143,-0.328571428571429,-0.314285714285714,
-0.3,-0.285714285714286,-0.271428571428571,-0.257142857142857,-0.242857142857143,
-0.228571428571429,-0.214285714285714,-0.2,-0.185714285714286,-0.171428571428571,
-0.157142857142857,-0.142857142857143,-0.128571428571429,-0.114285714285714,
-0.1,-0.0857142857142857,-0.0714285714285714,-0.0571428571428571,-0.0428571428571429,
-0.0285714285714286,-0.0142857142857143,0.),(0.,2.1),.UNSPECIFIED.);
#214=B_SPLINE_SURFACE_WITH_KNOTS('',5,1,((#14235,#14236),(#14237,#14238),
(#14239,#14240),(#14241,#14242),(#14243,#14244),(#14245,#14246),(#14247,
#14248),(#14249,#14250),(#14251,#14252),(#14253,#14254),(#14255,#14256),
(#14257,#14258),(#14259,#14260),(#14261,#14262),(#14263,#14264),(#14265,
#14266),(#14267,#14268),(#14269,#14270),(#14271,#14272),(#14273,#14274),
(#14275,#14276),(#14277,#14278),(#14279,#14280),(#14281,#14282),(#14283,
#14284),(#14285,#14286),(#14287,#14288),(#14289,#14290),(#14291,#14292),
(#14293,#14294),(#14295,#14296),(#14297,#14298),(#14299,#14300),(#14301,
#14302),(#14303,#14304),(#14305,#14306),(#14307,#14308),(#14309,#14310),
(#14311,#14312),(#14313,#14314),(#14315,#14316),(#14317,#14318),(#14319,
#14320),(#14321,#14322),(#14323,#14324),(#14325,#14326),(#14327,#14328),
(#14329,#14330),(#14331,#14332),(#14333,#14334),(#14335,#14336),(#14337,
#14338),(#14339,#14340),(#14341,#14342),(#14343,#14344),(#14345,#14346),
(#14347,#14348),(#14349,#14350),(#14351,#14352),(#14353,#14354),(#14355,
#14356),(#14357,#14358),(#14359,#14360),(#14361,#14362),(#14363,#14364),
(#14365,#14366),(#14367,#14368),(#14369,#14370),(#14371,#14372),(#14373,
#14374),(#14375,#14376),(#14377,#14378),(#14379,#14380),(#14381,#14382),
(#14383,#14384)),.UNSPECIFIED.,.F.,.F.,.F.,(6,1,1,1,1,1,1,1,1,1,1,1,1,1,
1,1,1,1,1,1,1,1,1,1,1,1,1,1,1,1,1,1,1,1,1,1,1,1,1,1,1,1,1,1,1,1,1,1,1,1,
1,1,1,1,1,1,1,1,1,1,1,1,1,1,1,1,1,1,1,1,6),(2,2),(0.,0.0142857142857143,
0.0285714285714286,0.0428571428571429,0.0571428571428571,0.0714285714285714,
0.0857142857142857,0.1,0.114285714285714,0.128571428571429,0.142857142857143,
0.157142857142857,0.171428571428571,0.185714285714286,0.2,0.214285714285714,
0.228571428571429,0.242857142857143,0.257142857142857,0.271428571428571,
0.285714285714286,0.3,0.314285714285714,0.328571428571429,0.342857142857143,
0.357142857142857,0.371428571428571,0.385714285714286,0.4,0.414285714285714,
0.428571428571429,0.442857142857143,0.457142857142857,0.471428571428572,
0.485714285714286,0.5,0.514285714285714,0.528571428571429,0.542857142857143,
0.557142857142857,0.571428571428571,0.585714285714286,0.6,0.614285714285714,
0.628571428571428,0.642857142857142,0.657142857142857,0.671428571428571,
0.685714285714285,0.699999999999999,0.714285714285714,0.728571428571428,
0.742857142857142,0.757142857142856,0.771428571428571,0.785714285714285,
0.799999999999999,0.814285714285713,0.828571428571428,0.842857142857142,
0.857142857142856,0.87142857142857,0.885714285714284,0.899999999999999,
0.914285714285713,0.928571428571427,0.942857142857141,0.957142857142856,
0.97142857142857,0.985714285714284,1.),(0.,2.1),.UNSPECIFIED.);
#215=B_SPLINE_SURFACE_WITH_KNOTS('',5,1,((#14529,#14530),(#14531,#14532),
(#14533,#14534),(#14535,#14536),(#14537,#14538),(#14539,#14540),(#14541,
#14542),(#14543,#14544),(#14545,#14546),(#14547,#14548),(#14549,#14550),
(#14551,#14552),(#14553,#14554),(#14555,#14556),(#14557,#14558),(#14559,
#14560),(#14561,#14562),(#14563,#14564),(#14565,#14566),(#14567,#14568),
(#14569,#14570),(#14571,#14572),(#14573,#14574),(#14575,#14576),(#14577,
#14578),(#14579,#14580),(#14581,#14582),(#14583,#14584),(#14585,#14586),
(#14587,#14588),(#14589,#14590),(#14591,#14592),(#14593,#14594),(#14595,
#14596),(#14597,#14598),(#14599,#14600),(#14601,#14602),(#14603,#14604),
(#14605,#14606),(#14607,#14608),(#14609,#14610),(#14611,#14612),(#14613,
#14614),(#14615,#14616),(#14617,#14618),(#14619,#14620),(#14621,#14622),
(#14623,#14624),(#14625,#14626),(#14627,#14628),(#14629,#14630),(#14631,
#14632),(#14633,#14634),(#14635,#14636),(#14637,#14638),(#14639,#14640),
(#14641,#14642),(#14643,#14644),(#14645,#14646),(#14647,#14648),(#14649,
#14650),(#14651,#14652),(#14653,#14654),(#14655,#14656),(#14657,#14658),
(#14659,#14660),(#14661,#14662),(#14663,#14664),(#14665,#14666),(#14667,
#14668),(#14669,#14670),(#14671,#14672),(#14673,#14674),(#14675,#14676),
(#14677,#14678)),.UNSPECIFIED.,.F.,.F.,.F.,(6,1,1,1,1,1,1,1,1,1,1,1,1,1,
1,1,1,1,1,1,1,1,1,1,1,1,1,1,1,1,1,1,1,1,1,1,1,1,1,1,1,1,1,1,1,1,1,1,1,1,
1,1,1,1,1,1,1,1,1,1,1,1,1,1,1,1,1,1,1,1,6),(2,2),(-1.,-0.985714285714284,
-0.97142857142857,-0.957142857142856,-0.942857142857141,-0.928571428571427,
-0.914285714285713,-0.899999999999999,-0.885714285714284,-0.87142857142857,
-0.857142857142856,-0.842857142857142,-0.828571428571428,-0.814285714285713,
-0.799999999999999,-0.785714285714285,-0.771428571428571,-0.757142857142856,
-0.742857142857142,-0.728571428571428,-0.714285714285714,-0.699999999999999,
-0.685714285714285,-0.671428571428571,-0.657142857142857,-0.642857142857142,
-0.628571428571428,-0.614285714285714,-0.6,-0.585714285714286,-0.571428571428571,
-0.557142857142857,-0.542857142857143,-0.528571428571429,-0.514285714285714,
-0.5,-0.485714285714286,-0.471428571428572,-0.457142857142857,-0.442857142857143,
-0.428571428571429,-0.414285714285714,-0.4,-0.385714285714286,-0.371428571428571,
-0.357142857142857,-0.342857142857143,-0.328571428571429,-0.314285714285714,
-0.3,-0.285714285714286,-0.271428571428571,-0.257142857142857,-0.242857142857143,
-0.228571428571429,-0.214285714285714,-0.2,-0.185714285714286,-0.171428571428571,
-0.157142857142857,-0.142857142857143,-0.128571428571429,-0.114285714285714,
-0.1,-0.0857142857142857,-0.0714285714285714,-0.0571428571428571,-0.0428571428571429,
-0.0285714285714286,-0.0142857142857143,0.),(0.,2.1),.UNSPECIFIED.);
#216=B_SPLINE_SURFACE_WITH_KNOTS('',5,1,((#14829,#14830),(#14831,#14832),
(#14833,#14834),(#14835,#14836),(#14837,#14838),(#14839,#14840),(#14841,
#14842),(#14843,#14844),(#14845,#14846),(#14847,#14848),(#14849,#14850),
(#14851,#14852),(#14853,#14854),(#14855,#14856),(#14857,#14858),(#14859,
#14860),(#14861,#14862),(#14863,#14864),(#14865,#14866),(#14867,#14868),
(#14869,#14870),(#14871,#14872),(#14873,#14874),(#14875,#14876),(#14877,
#14878),(#14879,#14880),(#14881,#14882),(#14883,#14884),(#14885,#14886),
(#14887,#14888),(#14889,#14890),(#14891,#14892),(#14893,#14894),(#14895,
#14896),(#14897,#14898),(#14899,#14900),(#14901,#14902),(#14903,#14904),
(#14905,#14906),(#14907,#14908),(#14909,#14910),(#14911,#14912),(#14913,
#14914),(#14915,#14916),(#14917,#14918),(#14919,#14920),(#14921,#14922),
(#14923,#14924),(#14925,#14926),(#14927,#14928),(#14929,#14930),(#14931,
#14932),(#14933,#14934),(#14935,#14936),(#14937,#14938),(#14939,#14940),
(#14941,#14942),(#14943,#14944),(#14945,#14946),(#14947,#14948),(#14949,
#14950),(#14951,#14952),(#14953,#14954),(#14955,#14956),(#14957,#14958),
(#14959,#14960),(#14961,#14962),(#14963,#14964),(#14965,#14966),(#14967,
#14968),(#14969,#14970),(#14971,#14972),(#14973,#14974),(#14975,#14976),
(#14977,#14978)),.UNSPECIFIED.,.F.,.F.,.F.,(6,1,1,1,1,1,1,1,1,1,1,1,1,1,
1,1,1,1,1,1,1,1,1,1,1,1,1,1,1,1,1,1,1,1,1,1,1,1,1,1,1,1,1,1,1,1,1,1,1,1,
1,1,1,1,1,1,1,1,1,1,1,1,1,1,1,1,1,1,1,1,6),(2,2),(0.,0.0142857142857143,
0.0285714285714286,0.0428571428571429,0.0571428571428571,0.0714285714285714,
0.0857142857142857,0.1,0.114285714285714,0.128571428571429,0.142857142857143,
0.157142857142857,0.171428571428571,0.185714285714286,0.2,0.214285714285714,
0.228571428571429,0.242857142857143,0.257142857142857,0.271428571428571,
0.285714285714286,0.3,0.314285714285714,0.328571428571429,0.342857142857143,
0.357142857142857,0.371428571428571,0.385714285714286,0.4,0.414285714285714,
0.428571428571429,0.442857142857143,0.457142857142857,0.471428571428572,
0.485714285714286,0.5,0.514285714285714,0.528571428571429,0.542857142857143,
0.557142857142857,0.571428571428571,0.585714285714286,0.6,0.614285714285714,
0.628571428571428,0.642857142857142,0.657142857142857,0.671428571428571,
0.685714285714285,0.699999999999999,0.714285714285714,0.728571428571428,
0.742857142857142,0.757142857142856,0.771428571428571,0.785714285714285,
0.799999999999999,0.814285714285713,0.828571428571428,0.842857142857142,
0.857142857142856,0.87142857142857,0.885714285714284,0.899999999999999,
0.914285714285713,0.928571428571427,0.942857142857141,0.957142857142856,
0.97142857142857,0.985714285714284,1.),(0.,2.1),.UNSPECIFIED.);
#217=B_SPLINE_SURFACE_WITH_KNOTS('',5,1,((#15123,#15124),(#15125,#15126),
(#15127,#15128),(#15129,#15130),(#15131,#15132),(#15133,#15134),(#15135,
#15136),(#15137,#15138),(#15139,#15140),(#15141,#15142),(#15143,#15144),
(#15145,#15146),(#15147,#15148),(#15149,#15150),(#15151,#15152),(#15153,
#15154),(#15155,#15156),(#15157,#15158),(#15159,#15160),(#15161,#15162),
(#15163,#15164),(#15165,#15166),(#15167,#15168),(#15169,#15170),(#15171,
#15172),(#15173,#15174),(#15175,#15176),(#15177,#15178),(#15179,#15180),
(#15181,#15182),(#15183,#15184),(#15185,#15186),(#15187,#15188),(#15189,
#15190),(#15191,#15192),(#15193,#15194),(#15195,#15196),(#15197,#15198),
(#15199,#15200),(#15201,#15202),(#15203,#15204),(#15205,#15206),(#15207,
#15208),(#15209,#15210),(#15211,#15212),(#15213,#15214),(#15215,#15216),
(#15217,#15218),(#15219,#15220),(#15221,#15222),(#15223,#15224),(#15225,
#15226),(#15227,#15228),(#15229,#15230),(#15231,#15232),(#15233,#15234),
(#15235,#15236),(#15237,#15238),(#15239,#15240),(#15241,#15242),(#15243,
#15244),(#15245,#15246),(#15247,#15248),(#15249,#15250),(#15251,#15252),
(#15253,#15254),(#15255,#15256),(#15257,#15258),(#15259,#15260),(#15261,
#15262),(#15263,#15264),(#15265,#15266),(#15267,#15268),(#15269,#15270),
(#15271,#15272)),.UNSPECIFIED.,.F.,.F.,.F.,(6,1,1,1,1,1,1,1,1,1,1,1,1,1,
1,1,1,1,1,1,1,1,1,1,1,1,1,1,1,1,1,1,1,1,1,1,1,1,1,1,1,1,1,1,1,1,1,1,1,1,
1,1,1,1,1,1,1,1,1,1,1,1,1,1,1,1,1,1,1,1,6),(2,2),(-1.,-0.985714285714284,
-0.97142857142857,-0.957142857142856,-0.942857142857141,-0.928571428571427,
-0.914285714285713,-0.899999999999999,-0.885714285714284,-0.87142857142857,
-0.857142857142856,-0.842857142857142,-0.828571428571428,-0.814285714285713,
-0.799999999999999,-0.785714285714285,-0.771428571428571,-0.757142857142856,
-0.742857142857142,-0.728571428571428,-0.714285714285714,-0.699999999999999,
-0.685714285714285,-0.671428571428571,-0.657142857142857,-0.642857142857142,
-0.628571428571428,-0.614285714285714,-0.6,-0.585714285714286,-0.571428571428571,
-0.557142857142857,-0.542857142857143,-0.528571428571429,-0.514285714285714,
-0.5,-0.485714285714286,-0.471428571428572,-0.457142857142857,-0.442857142857143,
-0.428571428571429,-0.414285714285714,-0.4,-0.385714285714286,-0.371428571428571,
-0.357142857142857,-0.342857142857143,-0.328571428571429,-0.314285714285714,
-0.3,-0.285714285714286,-0.271428571428571,-0.257142857142857,-0.242857142857143,
-0.228571428571429,-0.214285714285714,-0.2,-0.185714285714286,-0.171428571428571,
-0.157142857142857,-0.142857142857143,-0.128571428571429,-0.114285714285714,
-0.1,-0.0857142857142857,-0.0714285714285714,-0.0571428571428571,-0.0428571428571429,
-0.0285714285714286,-0.0142857142857143,0.),(0.,2.1),.UNSPECIFIED.);
#218=B_SPLINE_SURFACE_WITH_KNOTS('',5,1,((#15423,#15424),(#15425,#15426),
(#15427,#15428),(#15429,#15430),(#15431,#15432),(#15433,#15434),(#15435,
#15436),(#15437,#15438),(#15439,#15440),(#15441,#15442),(#15443,#15444),
(#15445,#15446),(#15447,#15448),(#15449,#15450),(#15451,#15452),(#15453,
#15454),(#15455,#15456),(#15457,#15458),(#15459,#15460),(#15461,#15462),
(#15463,#15464),(#15465,#15466),(#15467,#15468),(#15469,#15470),(#15471,
#15472),(#15473,#15474),(#15475,#15476),(#15477,#15478),(#15479,#15480),
(#15481,#15482),(#15483,#15484),(#15485,#15486),(#15487,#15488),(#15489,
#15490),(#15491,#15492),(#15493,#15494),(#15495,#15496),(#15497,#15498),
(#15499,#15500),(#15501,#15502),(#15503,#15504),(#15505,#15506),(#15507,
#15508),(#15509,#15510),(#15511,#15512),(#15513,#15514),(#15515,#15516),
(#15517,#15518),(#15519,#15520),(#15521,#15522),(#15523,#15524),(#15525,
#15526),(#15527,#15528),(#15529,#15530),(#15531,#15532),(#15533,#15534),
(#15535,#15536),(#15537,#15538),(#15539,#15540),(#15541,#15542),(#15543,
#15544),(#15545,#15546),(#15547,#15548),(#15549,#15550),(#15551,#15552),
(#15553,#15554),(#15555,#15556),(#15557,#15558),(#15559,#15560),(#15561,
#15562),(#15563,#15564),(#15565,#15566),(#15567,#15568),(#15569,#15570),
(#15571,#15572)),.UNSPECIFIED.,.F.,.F.,.F.,(6,1,1,1,1,1,1,1,1,1,1,1,1,1,
1,1,1,1,1,1,1,1,1,1,1,1,1,1,1,1,1,1,1,1,1,1,1,1,1,1,1,1,1,1,1,1,1,1,1,1,
1,1,1,1,1,1,1,1,1,1,1,1,1,1,1,1,1,1,1,1,6),(2,2),(0.,0.0142857142857143,
0.0285714285714286,0.0428571428571429,0.0571428571428571,0.0714285714285714,
0.0857142857142857,0.1,0.114285714285714,0.128571428571429,0.142857142857143,
0.157142857142857,0.171428571428571,0.185714285714286,0.2,0.214285714285714,
0.228571428571429,0.242857142857143,0.257142857142857,0.271428571428571,
0.285714285714286,0.3,0.314285714285714,0.328571428571429,0.342857142857143,
0.357142857142857,0.371428571428571,0.385714285714286,0.4,0.414285714285714,
0.428571428571429,0.442857142857143,0.457142857142857,0.471428571428572,
0.485714285714286,0.5,0.514285714285714,0.528571428571429,0.542857142857143,
0.557142857142857,0.571428571428571,0.585714285714286,0.6,0.614285714285714,
0.628571428571428,0.642857142857142,0.657142857142857,0.671428571428571,
0.685714285714285,0.699999999999999,0.714285714285714,0.728571428571428,
0.742857142857142,0.757142857142856,0.771428571428571,0.785714285714285,
0.799999999999999,0.814285714285713,0.828571428571428,0.842857142857142,
0.857142857142856,0.87142857142857,0.885714285714284,0.899999999999999,
0.914285714285713,0.928571428571427,0.942857142857141,0.957142857142856,
0.97142857142857,0.985714285714284,1.),(0.,2.1),.UNSPECIFIED.);
#219=B_SPLINE_SURFACE_WITH_KNOTS('',5,1,((#15717,#15718),(#15719,#15720),
(#15721,#15722),(#15723,#15724),(#15725,#15726),(#15727,#15728),(#15729,
#15730),(#15731,#15732),(#15733,#15734),(#15735,#15736),(#15737,#15738),
(#15739,#15740),(#15741,#15742),(#15743,#15744),(#15745,#15746),(#15747,
#15748),(#15749,#15750),(#15751,#15752),(#15753,#15754),(#15755,#15756),
(#15757,#15758),(#15759,#15760),(#15761,#15762),(#15763,#15764),(#15765,
#15766),(#15767,#15768),(#15769,#15770),(#15771,#15772),(#15773,#15774),
(#15775,#15776),(#15777,#15778),(#15779,#15780),(#15781,#15782),(#15783,
#15784),(#15785,#15786),(#15787,#15788),(#15789,#15790),(#15791,#15792),
(#15793,#15794),(#15795,#15796),(#15797,#15798),(#15799,#15800),(#15801,
#15802),(#15803,#15804),(#15805,#15806),(#15807,#15808),(#15809,#15810),
(#15811,#15812),(#15813,#15814),(#15815,#15816),(#15817,#15818),(#15819,
#15820),(#15821,#15822),(#15823,#15824),(#15825,#15826),(#15827,#15828),
(#15829,#15830),(#15831,#15832),(#15833,#15834),(#15835,#15836),(#15837,
#15838),(#15839,#15840),(#15841,#15842),(#15843,#15844),(#15845,#15846),
(#15847,#15848),(#15849,#15850),(#15851,#15852),(#15853,#15854),(#15855,
#15856),(#15857,#15858),(#15859,#15860),(#15861,#15862),(#15863,#15864),
(#15865,#15866)),.UNSPECIFIED.,.F.,.F.,.F.,(6,1,1,1,1,1,1,1,1,1,1,1,1,1,
1,1,1,1,1,1,1,1,1,1,1,1,1,1,1,1,1,1,1,1,1,1,1,1,1,1,1,1,1,1,1,1,1,1,1,1,
1,1,1,1,1,1,1,1,1,1,1,1,1,1,1,1,1,1,1,1,6),(2,2),(-1.,-0.985714285714284,
-0.97142857142857,-0.957142857142856,-0.942857142857141,-0.928571428571427,
-0.914285714285713,-0.899999999999999,-0.885714285714284,-0.87142857142857,
-0.857142857142856,-0.842857142857142,-0.828571428571428,-0.814285714285713,
-0.799999999999999,-0.785714285714285,-0.771428571428571,-0.757142857142856,
-0.742857142857142,-0.728571428571428,-0.714285714285714,-0.699999999999999,
-0.685714285714285,-0.671428571428571,-0.657142857142857,-0.642857142857142,
-0.628571428571428,-0.614285714285714,-0.6,-0.585714285714286,-0.571428571428571,
-0.557142857142857,-0.542857142857143,-0.528571428571429,-0.514285714285714,
-0.5,-0.485714285714286,-0.471428571428572,-0.457142857142857,-0.442857142857143,
-0.428571428571429,-0.414285714285714,-0.4,-0.385714285714286,-0.371428571428571,
-0.357142857142857,-0.342857142857143,-0.328571428571429,-0.314285714285714,
-0.3,-0.285714285714286,-0.271428571428571,-0.257142857142857,-0.242857142857143,
-0.228571428571429,-0.214285714285714,-0.2,-0.185714285714286,-0.171428571428571,
-0.157142857142857,-0.142857142857143,-0.128571428571429,-0.114285714285714,
-0.1,-0.0857142857142857,-0.0714285714285714,-0.0571428571428571,-0.0428571428571429,
-0.0285714285714286,-0.0142857142857143,0.),(0.,2.1),.UNSPECIFIED.);
#220=B_SPLINE_SURFACE_WITH_KNOTS('',5,1,((#16017,#16018),(#16019,#16020),
(#16021,#16022),(#16023,#16024),(#16025,#16026),(#16027,#16028),(#16029,
#16030),(#16031,#16032),(#16033,#16034),(#16035,#16036),(#16037,#16038),
(#16039,#16040),(#16041,#16042),(#16043,#16044),(#16045,#16046),(#16047,
#16048),(#16049,#16050),(#16051,#16052),(#16053,#16054),(#16055,#16056),
(#16057,#16058),(#16059,#16060),(#16061,#16062),(#16063,#16064),(#16065,
#16066),(#16067,#16068),(#16069,#16070),(#16071,#16072),(#16073,#16074),
(#16075,#16076),(#16077,#16078),(#16079,#16080),(#16081,#16082),(#16083,
#16084),(#16085,#16086),(#16087,#16088),(#16089,#16090),(#16091,#16092),
(#16093,#16094),(#16095,#16096),(#16097,#16098),(#16099,#16100),(#16101,
#16102),(#16103,#16104),(#16105,#16106),(#16107,#16108),(#16109,#16110),
(#16111,#16112),(#16113,#16114),(#16115,#16116),(#16117,#16118),(#16119,
#16120),(#16121,#16122),(#16123,#16124),(#16125,#16126),(#16127,#16128),
(#16129,#16130),(#16131,#16132),(#16133,#16134),(#16135,#16136),(#16137,
#16138),(#16139,#16140),(#16141,#16142),(#16143,#16144),(#16145,#16146),
(#16147,#16148),(#16149,#16150),(#16151,#16152),(#16153,#16154),(#16155,
#16156),(#16157,#16158),(#16159,#16160),(#16161,#16162),(#16163,#16164),
(#16165,#16166)),.UNSPECIFIED.,.F.,.F.,.F.,(6,1,1,1,1,1,1,1,1,1,1,1,1,1,
1,1,1,1,1,1,1,1,1,1,1,1,1,1,1,1,1,1,1,1,1,1,1,1,1,1,1,1,1,1,1,1,1,1,1,1,
1,1,1,1,1,1,1,1,1,1,1,1,1,1,1,1,1,1,1,1,6),(2,2),(0.,0.0142857142857143,
0.0285714285714286,0.0428571428571429,0.0571428571428571,0.0714285714285714,
0.0857142857142857,0.1,0.114285714285714,0.128571428571429,0.142857142857143,
0.157142857142857,0.171428571428571,0.185714285714286,0.2,0.214285714285714,
0.228571428571429,0.242857142857143,0.257142857142857,0.271428571428571,
0.285714285714286,0.3,0.314285714285714,0.328571428571429,0.342857142857143,
0.357142857142857,0.371428571428571,0.385714285714286,0.4,0.414285714285714,
0.428571428571429,0.442857142857143,0.457142857142857,0.471428571428572,
0.485714285714286,0.5,0.514285714285714,0.528571428571429,0.542857142857143,
0.557142857142857,0.571428571428571,0.585714285714286,0.6,0.614285714285714,
0.628571428571428,0.642857142857142,0.657142857142857,0.671428571428571,
0.685714285714285,0.699999999999999,0.714285714285714,0.728571428571428,
0.742857142857142,0.757142857142856,0.771428571428571,0.785714285714285,
0.799999999999999,0.814285714285713,0.828571428571428,0.842857142857142,
0.857142857142856,0.87142857142857,0.885714285714284,0.899999999999999,
0.914285714285713,0.928571428571427,0.942857142857141,0.957142857142856,
0.97142857142857,0.985714285714284,1.),(0.,2.1),.UNSPECIFIED.);
#221=B_SPLINE_SURFACE_WITH_KNOTS('',5,1,((#16311,#16312),(#16313,#16314),
(#16315,#16316),(#16317,#16318),(#16319,#16320),(#16321,#16322),(#16323,
#16324),(#16325,#16326),(#16327,#16328),(#16329,#16330),(#16331,#16332),
(#16333,#16334),(#16335,#16336),(#16337,#16338),(#16339,#16340),(#16341,
#16342),(#16343,#16344),(#16345,#16346),(#16347,#16348),(#16349,#16350),
(#16351,#16352),(#16353,#16354),(#16355,#16356),(#16357,#16358),(#16359,
#16360),(#16361,#16362),(#16363,#16364),(#16365,#16366),(#16367,#16368),
(#16369,#16370),(#16371,#16372),(#16373,#16374),(#16375,#16376),(#16377,
#16378),(#16379,#16380),(#16381,#16382),(#16383,#16384),(#16385,#16386),
(#16387,#16388),(#16389,#16390),(#16391,#16392),(#16393,#16394),(#16395,
#16396),(#16397,#16398),(#16399,#16400),(#16401,#16402),(#16403,#16404),
(#16405,#16406),(#16407,#16408),(#16409,#16410),(#16411,#16412),(#16413,
#16414),(#16415,#16416),(#16417,#16418),(#16419,#16420),(#16421,#16422),
(#16423,#16424),(#16425,#16426),(#16427,#16428),(#16429,#16430),(#16431,
#16432),(#16433,#16434),(#16435,#16436),(#16437,#16438),(#16439,#16440),
(#16441,#16442),(#16443,#16444),(#16445,#16446),(#16447,#16448),(#16449,
#16450),(#16451,#16452),(#16453,#16454),(#16455,#16456),(#16457,#16458),
(#16459,#16460)),.UNSPECIFIED.,.F.,.F.,.F.,(6,1,1,1,1,1,1,1,1,1,1,1,1,1,
1,1,1,1,1,1,1,1,1,1,1,1,1,1,1,1,1,1,1,1,1,1,1,1,1,1,1,1,1,1,1,1,1,1,1,1,
1,1,1,1,1,1,1,1,1,1,1,1,1,1,1,1,1,1,1,1,6),(2,2),(-1.,-0.985714285714284,
-0.97142857142857,-0.957142857142856,-0.942857142857141,-0.928571428571427,
-0.914285714285713,-0.899999999999999,-0.885714285714284,-0.87142857142857,
-0.857142857142856,-0.842857142857142,-0.828571428571428,-0.814285714285713,
-0.799999999999999,-0.785714285714285,-0.771428571428571,-0.757142857142856,
-0.742857142857142,-0.728571428571428,-0.714285714285714,-0.699999999999999,
-0.685714285714285,-0.671428571428571,-0.657142857142857,-0.642857142857142,
-0.628571428571428,-0.614285714285714,-0.6,-0.585714285714286,-0.571428571428571,
-0.557142857142857,-0.542857142857143,-0.528571428571429,-0.514285714285714,
-0.5,-0.485714285714286,-0.471428571428572,-0.457142857142857,-0.442857142857143,
-0.428571428571429,-0.414285714285714,-0.4,-0.385714285714286,-0.371428571428571,
-0.357142857142857,-0.342857142857143,-0.328571428571429,-0.314285714285714,
-0.3,-0.285714285714286,-0.271428571428571,-0.257142857142857,-0.242857142857143,
-0.228571428571429,-0.214285714285714,-0.2,-0.185714285714286,-0.171428571428571,
-0.157142857142857,-0.142857142857143,-0.128571428571429,-0.114285714285714,
-0.1,-0.0857142857142857,-0.0714285714285714,-0.0571428571428571,-0.0428571428571429,
-0.0285714285714286,-0.0142857142857143,0.),(0.,2.1),.UNSPECIFIED.);
#222=B_SPLINE_SURFACE_WITH_KNOTS('',5,1,((#16611,#16612),(#16613,#16614),
(#16615,#16616),(#16617,#16618),(#16619,#16620),(#16621,#16622),(#16623,
#16624),(#16625,#16626),(#16627,#16628),(#16629,#16630),(#16631,#16632),
(#16633,#16634),(#16635,#16636),(#16637,#16638),(#16639,#16640),(#16641,
#16642),(#16643,#16644),(#16645,#16646),(#16647,#16648),(#16649,#16650),
(#16651,#16652),(#16653,#16654),(#16655,#16656),(#16657,#16658),(#16659,
#16660),(#16661,#16662),(#16663,#16664),(#16665,#16666),(#16667,#16668),
(#16669,#16670),(#16671,#16672),(#16673,#16674),(#16675,#16676),(#16677,
#16678),(#16679,#16680),(#16681,#16682),(#16683,#16684),(#16685,#16686),
(#16687,#16688),(#16689,#16690),(#16691,#16692),(#16693,#16694),(#16695,
#16696),(#16697,#16698),(#16699,#16700),(#16701,#16702),(#16703,#16704),
(#16705,#16706),(#16707,#16708),(#16709,#16710),(#16711,#16712),(#16713,
#16714),(#16715,#16716),(#16717,#16718),(#16719,#16720),(#16721,#16722),
(#16723,#16724),(#16725,#16726),(#16727,#16728),(#16729,#16730),(#16731,
#16732),(#16733,#16734),(#16735,#16736),(#16737,#16738),(#16739,#16740),
(#16741,#16742),(#16743,#16744),(#16745,#16746),(#16747,#16748),(#16749,
#16750),(#16751,#16752),(#16753,#16754),(#16755,#16756),(#16757,#16758),
(#16759,#16760)),.UNSPECIFIED.,.F.,.F.,.F.,(6,1,1,1,1,1,1,1,1,1,1,1,1,1,
1,1,1,1,1,1,1,1,1,1,1,1,1,1,1,1,1,1,1,1,1,1,1,1,1,1,1,1,1,1,1,1,1,1,1,1,
1,1,1,1,1,1,1,1,1,1,1,1,1,1,1,1,1,1,1,1,6),(2,2),(0.,0.0142857142857143,
0.0285714285714286,0.0428571428571429,0.0571428571428571,0.0714285714285714,
0.0857142857142857,0.1,0.114285714285714,0.128571428571429,0.142857142857143,
0.157142857142857,0.171428571428571,0.185714285714286,0.2,0.214285714285714,
0.228571428571429,0.242857142857143,0.257142857142857,0.271428571428571,
0.285714285714286,0.3,0.314285714285714,0.328571428571429,0.342857142857143,
0.357142857142857,0.371428571428571,0.385714285714286,0.4,0.414285714285714,
0.428571428571429,0.442857142857143,0.457142857142857,0.471428571428572,
0.485714285714286,0.5,0.514285714285714,0.528571428571429,0.542857142857143,
0.557142857142857,0.571428571428571,0.585714285714286,0.6,0.614285714285714,
0.628571428571428,0.642857142857142,0.657142857142857,0.671428571428571,
0.685714285714285,0.699999999999999,0.714285714285714,0.728571428571428,
0.742857142857142,0.757142857142856,0.771428571428571,0.785714285714285,
0.799999999999999,0.814285714285713,0.828571428571428,0.842857142857142,
0.857142857142856,0.87142857142857,0.885714285714284,0.899999999999999,
0.914285714285713,0.928571428571427,0.942857142857141,0.957142857142856,
0.97142857142857,0.985714285714284,1.),(0.,2.1),.UNSPECIFIED.);
#223=B_SPLINE_SURFACE_WITH_KNOTS('',5,1,((#16905,#16906),(#16907,#16908),
(#16909,#16910),(#16911,#16912),(#16913,#16914),(#16915,#16916),(#16917,
#16918),(#16919,#16920),(#16921,#16922),(#16923,#16924),(#16925,#16926),
(#16927,#16928),(#16929,#16930),(#16931,#16932),(#16933,#16934),(#16935,
#16936),(#16937,#16938),(#16939,#16940),(#16941,#16942),(#16943,#16944),
(#16945,#16946),(#16947,#16948),(#16949,#16950),(#16951,#16952),(#16953,
#16954),(#16955,#16956),(#16957,#16958),(#16959,#16960),(#16961,#16962),
(#16963,#16964),(#16965,#16966),(#16967,#16968),(#16969,#16970),(#16971,
#16972),(#16973,#16974),(#16975,#16976),(#16977,#16978),(#16979,#16980),
(#16981,#16982),(#16983,#16984),(#16985,#16986),(#16987,#16988),(#16989,
#16990),(#16991,#16992),(#16993,#16994),(#16995,#16996),(#16997,#16998),
(#16999,#17000),(#17001,#17002),(#17003,#17004),(#17005,#17006),(#17007,
#17008),(#17009,#17010),(#17011,#17012),(#17013,#17014),(#17015,#17016),
(#17017,#17018),(#17019,#17020),(#17021,#17022),(#17023,#17024),(#17025,
#17026),(#17027,#17028),(#17029,#17030),(#17031,#17032),(#17033,#17034),
(#17035,#17036),(#17037,#17038),(#17039,#17040),(#17041,#17042),(#17043,
#17044),(#17045,#17046),(#17047,#17048),(#17049,#17050),(#17051,#17052),
(#17053,#17054)),.UNSPECIFIED.,.F.,.F.,.F.,(6,1,1,1,1,1,1,1,1,1,1,1,1,1,
1,1,1,1,1,1,1,1,1,1,1,1,1,1,1,1,1,1,1,1,1,1,1,1,1,1,1,1,1,1,1,1,1,1,1,1,
1,1,1,1,1,1,1,1,1,1,1,1,1,1,1,1,1,1,1,1,6),(2,2),(-1.,-0.985714285714284,
-0.97142857142857,-0.957142857142856,-0.942857142857141,-0.928571428571427,
-0.914285714285713,-0.899999999999999,-0.885714285714284,-0.87142857142857,
-0.857142857142856,-0.842857142857142,-0.828571428571428,-0.814285714285713,
-0.799999999999999,-0.785714285714285,-0.771428571428571,-0.757142857142856,
-0.742857142857142,-0.728571428571428,-0.714285714285714,-0.699999999999999,
-0.685714285714285,-0.671428571428571,-0.657142857142857,-0.642857142857142,
-0.628571428571428,-0.614285714285714,-0.6,-0.585714285714286,-0.571428571428571,
-0.557142857142857,-0.542857142857143,-0.528571428571429,-0.514285714285714,
-0.5,-0.485714285714286,-0.471428571428572,-0.457142857142857,-0.442857142857143,
-0.428571428571429,-0.414285714285714,-0.4,-0.385714285714286,-0.371428571428571,
-0.357142857142857,-0.342857142857143,-0.328571428571429,-0.314285714285714,
-0.3,-0.285714285714286,-0.271428571428571,-0.257142857142857,-0.242857142857143,
-0.228571428571429,-0.214285714285714,-0.2,-0.185714285714286,-0.171428571428571,
-0.157142857142857,-0.142857142857143,-0.128571428571429,-0.114285714285714,
-0.1,-0.0857142857142857,-0.0714285714285714,-0.0571428571428571,-0.0428571428571429,
-0.0285714285714286,-0.0142857142857143,0.),(0.,2.1),.UNSPECIFIED.);
#224=B_SPLINE_SURFACE_WITH_KNOTS('',5,1,((#17220,#17221),(#17222,#17223),
(#17224,#17225),(#17226,#17227),(#17228,#17229),(#17230,#17231),(#17232,
#17233),(#17234,#17235),(#17236,#17237),(#17238,#17239),(#17240,#17241),
(#17242,#17243),(#17244,#17245),(#17246,#17247),(#17248,#17249),(#17250,
#17251),(#17252,#17253),(#17254,#17255),(#17256,#17257),(#17258,#17259),
(#17260,#17261),(#17262,#17263),(#17264,#17265),(#17266,#17267),(#17268,
#17269),(#17270,#17271),(#17272,#17273),(#17274,#17275),(#17276,#17277),
(#17278,#17279),(#17280,#17281),(#17282,#17283),(#17284,#17285),(#17286,
#17287),(#17288,#17289),(#17290,#17291),(#17292,#17293),(#17294,#17295),
(#17296,#17297),(#17298,#17299),(#17300,#17301),(#17302,#17303),(#17304,
#17305),(#17306,#17307),(#17308,#17309),(#17310,#17311),(#17312,#17313),
(#17314,#17315),(#17316,#17317),(#17318,#17319),(#17320,#17321),(#17322,
#17323),(#17324,#17325),(#17326,#17327),(#17328,#17329),(#17330,#17331),
(#17332,#17333),(#17334,#17335),(#17336,#17337),(#17338,#17339),(#17340,
#17341),(#17342,#17343),(#17344,#17345),(#17346,#17347),(#17348,#17349),
(#17350,#17351),(#17352,#17353),(#17354,#17355),(#17356,#17357),(#17358,
#17359),(#17360,#17361),(#17362,#17363),(#17364,#17365),(#17366,#17367),
(#17368,#17369)),.UNSPECIFIED.,.F.,.F.,.F.,(6,1,1,1,1,1,1,1,1,1,1,1,1,1,
1,1,1,1,1,1,1,1,1,1,1,1,1,1,1,1,1,1,1,1,1,1,1,1,1,1,1,1,1,1,1,1,1,1,1,1,
1,1,1,1,1,1,1,1,1,1,1,1,1,1,1,1,1,1,1,1,6),(2,2),(0.,0.0142857142857143,
0.0285714285714286,0.0428571428571429,0.0571428571428571,0.0714285714285714,
0.0857142857142857,0.1,0.114285714285714,0.128571428571429,0.142857142857143,
0.157142857142857,0.171428571428571,0.185714285714286,0.2,0.214285714285714,
0.228571428571429,0.242857142857143,0.257142857142857,0.271428571428571,
0.285714285714286,0.3,0.314285714285714,0.328571428571429,0.342857142857143,
0.357142857142857,0.371428571428571,0.385714285714286,0.4,0.414285714285714,
0.428571428571429,0.442857142857143,0.457142857142857,0.471428571428572,
0.485714285714286,0.5,0.514285714285714,0.528571428571429,0.542857142857143,
0.557142857142857,0.571428571428571,0.585714285714286,0.6,0.614285714285714,
0.628571428571428,0.642857142857142,0.657142857142857,0.671428571428571,
0.685714285714285,0.699999999999999,0.714285714285714,0.728571428571428,
0.742857142857142,0.757142857142856,0.771428571428571,0.785714285714285,
0.799999999999999,0.814285714285713,0.828571428571428,0.842857142857142,
0.857142857142856,0.87142857142857,0.885714285714284,0.899999999999999,
0.914285714285713,0.928571428571427,0.942857142857141,0.957142857142856,
0.97142857142857,0.985714285714284,1.),(0.,2.1),.UNSPECIFIED.);
#225=B_SPLINE_SURFACE_WITH_KNOTS('',5,1,((#17514,#17515),(#17516,#17517),
(#17518,#17519),(#17520,#17521),(#17522,#17523),(#17524,#17525),(#17526,
#17527),(#17528,#17529),(#17530,#17531),(#17532,#17533),(#17534,#17535),
(#17536,#17537),(#17538,#17539),(#17540,#17541),(#17542,#17543),(#17544,
#17545),(#17546,#17547),(#17548,#17549),(#17550,#17551),(#17552,#17553),
(#17554,#17555),(#17556,#17557),(#17558,#17559),(#17560,#17561),(#17562,
#17563),(#17564,#17565),(#17566,#17567),(#17568,#17569),(#17570,#17571),
(#17572,#17573),(#17574,#17575),(#17576,#17577),(#17578,#17579),(#17580,
#17581),(#17582,#17583),(#17584,#17585),(#17586,#17587),(#17588,#17589),
(#17590,#17591),(#17592,#17593),(#17594,#17595),(#17596,#17597),(#17598,
#17599),(#17600,#17601),(#17602,#17603),(#17604,#17605),(#17606,#17607),
(#17608,#17609),(#17610,#17611),(#17612,#17613),(#17614,#17615),(#17616,
#17617),(#17618,#17619),(#17620,#17621),(#17622,#17623),(#17624,#17625),
(#17626,#17627),(#17628,#17629),(#17630,#17631),(#17632,#17633),(#17634,
#17635),(#17636,#17637),(#17638,#17639),(#17640,#17641),(#17642,#17643),
(#17644,#17645),(#17646,#17647),(#17648,#17649),(#17650,#17651),(#17652,
#17653),(#17654,#17655),(#17656,#17657),(#17658,#17659),(#17660,#17661),
(#17662,#17663)),.UNSPECIFIED.,.F.,.F.,.F.,(6,1,1,1,1,1,1,1,1,1,1,1,1,1,
1,1,1,1,1,1,1,1,1,1,1,1,1,1,1,1,1,1,1,1,1,1,1,1,1,1,1,1,1,1,1,1,1,1,1,1,
1,1,1,1,1,1,1,1,1,1,1,1,1,1,1,1,1,1,1,1,6),(2,2),(-1.,-0.985714285714284,
-0.97142857142857,-0.957142857142856,-0.942857142857141,-0.928571428571427,
-0.914285714285713,-0.899999999999999,-0.885714285714284,-0.87142857142857,
-0.857142857142856,-0.842857142857142,-0.828571428571428,-0.814285714285713,
-0.799999999999999,-0.785714285714285,-0.771428571428571,-0.757142857142856,
-0.742857142857142,-0.728571428571428,-0.714285714285714,-0.699999999999999,
-0.685714285714285,-0.671428571428571,-0.657142857142857,-0.642857142857142,
-0.628571428571428,-0.614285714285714,-0.6,-0.585714285714286,-0.571428571428571,
-0.557142857142857,-0.542857142857143,-0.528571428571429,-0.514285714285714,
-0.5,-0.485714285714286,-0.471428571428572,-0.457142857142857,-0.442857142857143,
-0.428571428571429,-0.414285714285714,-0.4,-0.385714285714286,-0.371428571428571,
-0.357142857142857,-0.342857142857143,-0.328571428571429,-0.314285714285714,
-0.3,-0.285714285714286,-0.271428571428571,-0.257142857142857,-0.242857142857143,
-0.228571428571429,-0.214285714285714,-0.2,-0.185714285714286,-0.171428571428571,
-0.157142857142857,-0.142857142857143,-0.128571428571429,-0.114285714285714,
-0.1,-0.0857142857142857,-0.0714285714285714,-0.0571428571428571,-0.0428571428571429,
-0.0285714285714286,-0.0142857142857143,0.),(0.,2.1),.UNSPECIFIED.);
#226=B_SPLINE_SURFACE_WITH_KNOTS('',5,1,((#17814,#17815),(#17816,#17817),
(#17818,#17819),(#17820,#17821),(#17822,#17823),(#17824,#17825),(#17826,
#17827),(#17828,#17829),(#17830,#17831),(#17832,#17833),(#17834,#17835),
(#17836,#17837),(#17838,#17839),(#17840,#17841),(#17842,#17843),(#17844,
#17845),(#17846,#17847),(#17848,#17849),(#17850,#17851),(#17852,#17853),
(#17854,#17855),(#17856,#17857),(#17858,#17859),(#17860,#17861),(#17862,
#17863),(#17864,#17865),(#17866,#17867),(#17868,#17869),(#17870,#17871),
(#17872,#17873),(#17874,#17875),(#17876,#17877),(#17878,#17879),(#17880,
#17881),(#17882,#17883),(#17884,#17885),(#17886,#17887),(#17888,#17889),
(#17890,#17891),(#17892,#17893),(#17894,#17895),(#17896,#17897),(#17898,
#17899),(#17900,#17901),(#17902,#17903),(#17904,#17905),(#17906,#17907),
(#17908,#17909),(#17910,#17911),(#17912,#17913),(#17914,#17915),(#17916,
#17917),(#17918,#17919),(#17920,#17921),(#17922,#17923),(#17924,#17925),
(#17926,#17927),(#17928,#17929),(#17930,#17931),(#17932,#17933),(#17934,
#17935),(#17936,#17937),(#17938,#17939),(#17940,#17941),(#17942,#17943),
(#17944,#17945),(#17946,#17947),(#17948,#17949),(#17950,#17951),(#17952,
#17953),(#17954,#17955),(#17956,#17957),(#17958,#17959),(#17960,#17961),
(#17962,#17963)),.UNSPECIFIED.,.F.,.F.,.F.,(6,1,1,1,1,1,1,1,1,1,1,1,1,1,
1,1,1,1,1,1,1,1,1,1,1,1,1,1,1,1,1,1,1,1,1,1,1,1,1,1,1,1,1,1,1,1,1,1,1,1,
1,1,1,1,1,1,1,1,1,1,1,1,1,1,1,1,1,1,1,1,6),(2,2),(0.,0.0142857142857143,
0.0285714285714286,0.0428571428571429,0.0571428571428571,0.0714285714285714,
0.0857142857142857,0.1,0.114285714285714,0.128571428571429,0.142857142857143,
0.157142857142857,0.171428571428571,0.185714285714286,0.2,0.214285714285714,
0.228571428571429,0.242857142857143,0.257142857142857,0.271428571428571,
0.285714285714286,0.3,0.314285714285714,0.328571428571429,0.342857142857143,
0.357142857142857,0.371428571428571,0.385714285714286,0.4,0.414285714285714,
0.428571428571429,0.442857142857143,0.457142857142857,0.471428571428572,
0.485714285714286,0.5,0.514285714285714,0.528571428571429,0.542857142857143,
0.557142857142857,0.571428571428571,0.585714285714286,0.6,0.614285714285714,
0.628571428571428,0.642857142857142,0.657142857142857,0.671428571428571,
0.685714285714285,0.699999999999999,0.714285714285714,0.728571428571428,
0.742857142857142,0.757142857142856,0.771428571428571,0.785714285714285,
0.799999999999999,0.814285714285713,0.828571428571428,0.842857142857142,
0.857142857142856,0.87142857142857,0.885714285714284,0.899999999999999,
0.914285714285713,0.928571428571427,0.942857142857141,0.957142857142856,
0.97142857142857,0.985714285714284,1.),(0.,2.1),.UNSPECIFIED.);
#227=B_SPLINE_SURFACE_WITH_KNOTS('',5,1,((#18108,#18109),(#18110,#18111),
(#18112,#18113),(#18114,#18115),(#18116,#18117),(#18118,#18119),(#18120,
#18121),(#18122,#18123),(#18124,#18125),(#18126,#18127),(#18128,#18129),
(#18130,#18131),(#18132,#18133),(#18134,#18135),(#18136,#18137),(#18138,
#18139),(#18140,#18141),(#18142,#18143),(#18144,#18145),(#18146,#18147),
(#18148,#18149),(#18150,#18151),(#18152,#18153),(#18154,#18155),(#18156,
#18157),(#18158,#18159),(#18160,#18161),(#18162,#18163),(#18164,#18165),
(#18166,#18167),(#18168,#18169),(#18170,#18171),(#18172,#18173),(#18174,
#18175),(#18176,#18177),(#18178,#18179),(#18180,#18181),(#18182,#18183),
(#18184,#18185),(#18186,#18187),(#18188,#18189),(#18190,#18191),(#18192,
#18193),(#18194,#18195),(#18196,#18197),(#18198,#18199),(#18200,#18201),
(#18202,#18203),(#18204,#18205),(#18206,#18207),(#18208,#18209),(#18210,
#18211),(#18212,#18213),(#18214,#18215),(#18216,#18217),(#18218,#18219),
(#18220,#18221),(#18222,#18223),(#18224,#18225),(#18226,#18227),(#18228,
#18229),(#18230,#18231),(#18232,#18233),(#18234,#18235),(#18236,#18237),
(#18238,#18239),(#18240,#18241),(#18242,#18243),(#18244,#18245),(#18246,
#18247),(#18248,#18249),(#18250,#18251),(#18252,#18253),(#18254,#18255),
(#18256,#18257)),.UNSPECIFIED.,.F.,.F.,.F.,(6,1,1,1,1,1,1,1,1,1,1,1,1,1,
1,1,1,1,1,1,1,1,1,1,1,1,1,1,1,1,1,1,1,1,1,1,1,1,1,1,1,1,1,1,1,1,1,1,1,1,
1,1,1,1,1,1,1,1,1,1,1,1,1,1,1,1,1,1,1,1,6),(2,2),(-1.,-0.985714285714284,
-0.97142857142857,-0.957142857142856,-0.942857142857141,-0.928571428571427,
-0.914285714285713,-0.899999999999999,-0.885714285714284,-0.87142857142857,
-0.857142857142856,-0.842857142857142,-0.828571428571428,-0.814285714285713,
-0.799999999999999,-0.785714285714285,-0.771428571428571,-0.757142857142856,
-0.742857142857142,-0.728571428571428,-0.714285714285714,-0.699999999999999,
-0.685714285714285,-0.671428571428571,-0.657142857142857,-0.642857142857142,
-0.628571428571428,-0.614285714285714,-0.6,-0.585714285714286,-0.571428571428571,
-0.557142857142857,-0.542857142857143,-0.528571428571429,-0.514285714285714,
-0.5,-0.485714285714286,-0.471428571428572,-0.457142857142857,-0.442857142857143,
-0.428571428571429,-0.414285714285714,-0.4,-0.385714285714286,-0.371428571428571,
-0.357142857142857,-0.342857142857143,-0.328571428571429,-0.314285714285714,
-0.3,-0.285714285714286,-0.271428571428571,-0.257142857142857,-0.242857142857143,
-0.228571428571429,-0.214285714285714,-0.2,-0.185714285714286,-0.171428571428571,
-0.157142857142857,-0.142857142857143,-0.128571428571429,-0.114285714285714,
-0.1,-0.0857142857142857,-0.0714285714285714,-0.0571428571428571,-0.0428571428571429,
-0.0285714285714286,-0.0142857142857143,0.),(0.,2.1),.UNSPECIFIED.);
#228=B_SPLINE_SURFACE_WITH_KNOTS('',5,1,((#18408,#18409),(#18410,#18411),
(#18412,#18413),(#18414,#18415),(#18416,#18417),(#18418,#18419),(#18420,
#18421),(#18422,#18423),(#18424,#18425),(#18426,#18427),(#18428,#18429),
(#18430,#18431),(#18432,#18433),(#18434,#18435),(#18436,#18437),(#18438,
#18439),(#18440,#18441),(#18442,#18443),(#18444,#18445),(#18446,#18447),
(#18448,#18449),(#18450,#18451),(#18452,#18453),(#18454,#18455),(#18456,
#18457),(#18458,#18459),(#18460,#18461),(#18462,#18463),(#18464,#18465),
(#18466,#18467),(#18468,#18469),(#18470,#18471),(#18472,#18473),(#18474,
#18475),(#18476,#18477),(#18478,#18479),(#18480,#18481),(#18482,#18483),
(#18484,#18485),(#18486,#18487),(#18488,#18489),(#18490,#18491),(#18492,
#18493),(#18494,#18495),(#18496,#18497),(#18498,#18499),(#18500,#18501),
(#18502,#18503),(#18504,#18505),(#18506,#18507),(#18508,#18509),(#18510,
#18511),(#18512,#18513),(#18514,#18515),(#18516,#18517),(#18518,#18519),
(#18520,#18521),(#18522,#18523),(#18524,#18525),(#18526,#18527),(#18528,
#18529),(#18530,#18531),(#18532,#18533),(#18534,#18535),(#18536,#18537),
(#18538,#18539),(#18540,#18541),(#18542,#18543),(#18544,#18545),(#18546,
#18547),(#18548,#18549),(#18550,#18551),(#18552,#18553),(#18554,#18555),
(#18556,#18557)),.UNSPECIFIED.,.F.,.F.,.F.,(6,1,1,1,1,1,1,1,1,1,1,1,1,1,
1,1,1,1,1,1,1,1,1,1,1,1,1,1,1,1,1,1,1,1,1,1,1,1,1,1,1,1,1,1,1,1,1,1,1,1,
1,1,1,1,1,1,1,1,1,1,1,1,1,1,1,1,1,1,1,1,6),(2,2),(0.,0.0142857142857143,
0.0285714285714286,0.0428571428571429,0.0571428571428571,0.0714285714285714,
0.0857142857142857,0.1,0.114285714285714,0.128571428571429,0.142857142857143,
0.157142857142857,0.171428571428571,0.185714285714286,0.2,0.214285714285714,
0.228571428571429,0.242857142857143,0.257142857142857,0.271428571428571,
0.285714285714286,0.3,0.314285714285714,0.328571428571429,0.342857142857143,
0.357142857142857,0.371428571428571,0.385714285714286,0.4,0.414285714285714,
0.428571428571429,0.442857142857143,0.457142857142857,0.471428571428572,
0.485714285714286,0.5,0.514285714285714,0.528571428571429,0.542857142857143,
0.557142857142857,0.571428571428571,0.585714285714286,0.6,0.614285714285714,
0.628571428571428,0.642857142857142,0.657142857142857,0.671428571428571,
0.685714285714285,0.699999999999999,0.714285714285714,0.728571428571428,
0.742857142857142,0.757142857142856,0.771428571428571,0.785714285714285,
0.799999999999999,0.814285714285713,0.828571428571428,0.842857142857142,
0.857142857142856,0.87142857142857,0.885714285714284,0.899999999999999,
0.914285714285713,0.928571428571427,0.942857142857141,0.957142857142856,
0.97142857142857,0.985714285714284,1.),(0.,2.1),.UNSPECIFIED.);
#229=B_SPLINE_SURFACE_WITH_KNOTS('',5,1,((#19084,#19085),(#19086,#19087),
(#19088,#19089),(#19090,#19091),(#19092,#19093),(#19094,#19095),(#19096,
#19097),(#19098,#19099),(#19100,#19101),(#19102,#19103),(#19104,#19105),
(#19106,#19107),(#19108,#19109),(#19110,#19111),(#19112,#19113),(#19114,
#19115),(#19116,#19117),(#19118,#19119),(#19120,#19121),(#19122,#19123),
(#19124,#19125),(#19126,#19127),(#19128,#19129),(#19130,#19131),(#19132,
#19133),(#19134,#19135),(#19136,#19137),(#19138,#19139),(#19140,#19141),
(#19142,#19143),(#19144,#19145),(#19146,#19147),(#19148,#19149),(#19150,
#19151),(#19152,#19153),(#19154,#19155),(#19156,#19157),(#19158,#19159),
(#19160,#19161),(#19162,#19163),(#19164,#19165),(#19166,#19167),(#19168,
#19169),(#19170,#19171),(#19172,#19173),(#19174,#19175),(#19176,#19177),
(#19178,#19179),(#19180,#19181),(#19182,#19183),(#19184,#19185),(#19186,
#19187),(#19188,#19189),(#19190,#19191),(#19192,#19193),(#19194,#19195),
(#19196,#19197),(#19198,#19199),(#19200,#19201),(#19202,#19203),(#19204,
#19205),(#19206,#19207),(#19208,#19209),(#19210,#19211),(#19212,#19213),
(#19214,#19215),(#19216,#19217),(#19218,#19219),(#19220,#19221),(#19222,
#19223),(#19224,#19225),(#19226,#19227),(#19228,#19229),(#19230,#19231),
(#19232,#19233)),.UNSPECIFIED.,.F.,.F.,.F.,(6,1,1,1,1,1,1,1,1,1,1,1,1,1,
1,1,1,1,1,1,1,1,1,1,1,1,1,1,1,1,1,1,1,1,1,1,1,1,1,1,1,1,1,1,1,1,1,1,1,1,
1,1,1,1,1,1,1,1,1,1,1,1,1,1,1,1,1,1,1,1,6),(2,2),(-1.,-0.985714285714284,
-0.97142857142857,-0.957142857142856,-0.942857142857141,-0.928571428571427,
-0.914285714285713,-0.899999999999999,-0.885714285714284,-0.87142857142857,
-0.857142857142856,-0.842857142857142,-0.828571428571428,-0.814285714285713,
-0.799999999999999,-0.785714285714285,-0.771428571428571,-0.757142857142856,
-0.742857142857142,-0.728571428571428,-0.714285714285714,-0.699999999999999,
-0.685714285714285,-0.671428571428571,-0.657142857142857,-0.642857142857142,
-0.628571428571428,-0.614285714285714,-0.6,-0.585714285714286,-0.571428571428571,
-0.557142857142857,-0.542857142857143,-0.528571428571429,-0.514285714285714,
-0.5,-0.485714285714286,-0.471428571428572,-0.457142857142857,-0.442857142857143,
-0.428571428571429,-0.414285714285714,-0.4,-0.385714285714286,-0.371428571428571,
-0.357142857142857,-0.342857142857143,-0.328571428571429,-0.314285714285714,
-0.3,-0.285714285714286,-0.271428571428571,-0.257142857142857,-0.242857142857143,
-0.228571428571429,-0.214285714285714,-0.2,-0.185714285714286,-0.171428571428571,
-0.157142857142857,-0.142857142857143,-0.128571428571429,-0.114285714285714,
-0.1,-0.0857142857142857,-0.0714285714285714,-0.0571428571428571,-0.0428571428571429,
-0.0285714285714286,-0.0142857142857143,0.),(0.,2.1),.UNSPECIFIED.);
#230=B_SPLINE_SURFACE_WITH_KNOTS('',5,1,((#19237,#19238),(#19239,#19240),
(#19241,#19242),(#19243,#19244),(#19245,#19246),(#19247,#19248),(#19249,
#19250),(#19251,#19252),(#19253,#19254),(#19255,#19256),(#19257,#19258),
(#19259,#19260),(#19261,#19262),(#19263,#19264),(#19265,#19266),(#19267,
#19268),(#19269,#19270),(#19271,#19272),(#19273,#19274),(#19275,#19276),
(#19277,#19278),(#19279,#19280),(#19281,#19282),(#19283,#19284),(#19285,
#19286),(#19287,#19288),(#19289,#19290),(#19291,#19292),(#19293,#19294),
(#19295,#19296),(#19297,#19298),(#19299,#19300),(#19301,#19302),(#19303,
#19304),(#19305,#19306),(#19307,#19308),(#19309,#19310),(#19311,#19312),
(#19313,#19314),(#19315,#19316),(#19317,#19318),(#19319,#19320),(#19321,
#19322),(#19323,#19324),(#19325,#19326),(#19327,#19328),(#19329,#19330),
(#19331,#19332),(#19333,#19334),(#19335,#19336),(#19337,#19338),(#19339,
#19340),(#19341,#19342),(#19343,#19344),(#19345,#19346),(#19347,#19348),
(#19349,#19350),(#19351,#19352),(#19353,#19354),(#19355,#19356),(#19357,
#19358),(#19359,#19360),(#19361,#19362),(#19363,#19364),(#19365,#19366),
(#19367,#19368),(#19369,#19370),(#19371,#19372),(#19373,#19374),(#19375,
#19376),(#19377,#19378),(#19379,#19380),(#19381,#19382),(#19383,#19384),
(#19385,#19386)),.UNSPECIFIED.,.F.,.F.,.F.,(6,1,1,1,1,1,1,1,1,1,1,1,1,1,
1,1,1,1,1,1,1,1,1,1,1,1,1,1,1,1,1,1,1,1,1,1,1,1,1,1,1,1,1,1,1,1,1,1,1,1,
1,1,1,1,1,1,1,1,1,1,1,1,1,1,1,1,1,1,1,1,6),(2,2),(0.,0.0142857142857143,
0.0285714285714286,0.0428571428571429,0.0571428571428571,0.0714285714285714,
0.0857142857142857,0.1,0.114285714285714,0.128571428571429,0.142857142857143,
0.157142857142857,0.171428571428571,0.185714285714286,0.2,0.214285714285714,
0.228571428571429,0.242857142857143,0.257142857142857,0.271428571428571,
0.285714285714286,0.3,0.314285714285714,0.328571428571429,0.342857142857143,
0.357142857142857,0.371428571428571,0.385714285714286,0.4,0.414285714285714,
0.428571428571429,0.442857142857143,0.457142857142857,0.471428571428572,
0.485714285714286,0.5,0.514285714285714,0.528571428571429,0.542857142857143,
0.557142857142857,0.571428571428571,0.585714285714286,0.6,0.614285714285714,
0.628571428571428,0.642857142857142,0.657142857142857,0.671428571428571,
0.685714285714285,0.699999999999999,0.714285714285714,0.728571428571428,
0.742857142857142,0.757142857142856,0.771428571428571,0.785714285714285,
0.799999999999999,0.814285714285713,0.828571428571428,0.842857142857142,
0.857142857142856,0.87142857142857,0.885714285714284,0.899999999999999,
0.914285714285713,0.928571428571427,0.942857142857141,0.957142857142856,
0.97142857142857,0.985714285714284,1.),(0.,2.1),.UNSPECIFIED.);
#231=PLANE('',#4918);
#232=PLANE('',#4922);
#233=PLANE('',#4926);
#234=PLANE('',#4930);
#235=PLANE('',#4934);
#236=PLANE('',#4938);
#237=PLANE('',#4942);
#238=PLANE('',#4946);
#239=PLANE('',#4950);
#240=PLANE('',#4954);
#241=PLANE('',#4958);
#242=PLANE('',#4962);
#243=PLANE('',#4966);
#244=PLANE('',#4970);
#245=PLANE('',#4974);
#246=PLANE('',#4978);
#247=PLANE('',#4982);
#248=PLANE('',#4986);
#249=PLANE('',#4990);
#250=PLANE('',#4994);
#251=PLANE('',#4998);
#252=PLANE('',#5002);
#253=PLANE('',#5006);
#254=PLANE('',#5010);
#255=PLANE('',#5014);
#256=PLANE('',#5018);
#257=PLANE('',#5022);
#258=PLANE('',#5026);
#259=PLANE('',#5030);
#260=PLANE('',#5034);
#261=PLANE('',#5038);
#262=PLANE('',#5042);
#263=PLANE('',#5046);
#264=PLANE('',#5050);
#265=PLANE('',#5054);
#266=PLANE('',#5058);
#267=PLANE('',#5062);
#268=PLANE('',#5066);
#269=PLANE('',#5124);
#270=PLANE('',#5148);
#271=PLANE('',#5192);
#272=PLANE('',#5194);
#273=PLANE('',#5208);
#274=PLANE('',#5209);
#275=PLANE('',#5210);
#276=PLANE('',#5211);
#277=PLANE('',#5212);
#278=PLANE('',#5213);
#279=PLANE('',#5214);
#280=PLANE('',#5215);
#281=PLANE('',#5216);
#282=PLANE('',#5217);
#283=PLANE('',#5218);
#284=PLANE('',#5219);
#285=PLANE('',#5220);
#286=PLANE('',#5223);
#287=PLANE('',#5235);
#288=PLANE('',#5236);
#289=PLANE('',#5237);
#290=PLANE('',#5238);
#291=PLANE('',#5239);
#292=PLANE('',#5240);
#293=PLANE('',#5241);
#294=PLANE('',#5242);
#295=PLANE('',#5243);
#296=PLANE('',#5244);
#297=PLANE('',#5245);
#298=PLANE('',#5246);
#299=PLANE('',#5247);
#300=PLANE('',#5250);
#301=PLANE('',#5255);
#302=PLANE('',#5262);
#303=PLANE('',#5266);
#304=PLANE('',#5267);
#305=PLANE('',#5275);
#306=PLANE('',#5281);
#307=PLANE('',#5290);
#308=PLANE('',#5296);
#309=PLANE('',#5300);
#310=PLANE('',#5304);
#311=PLANE('',#5308);
#312=PLANE('',#5325);
#313=PLANE('',#5328);
#314=PLANE('',#5334);
#315=PLANE('',#5348);
#316=PLANE('',#5374);
#317=PLANE('',#5377);
#318=PLANE('',#5383);
#319=PLANE('',#5397);
#320=PLANE('',#5405);
#321=PLANE('',#5406);
#322=PLANE('',#5407);
#323=PLANE('',#5411);
#324=PLANE('',#5415);
#325=FACE_OUTER_BOUND('',#601,.T.);
#326=FACE_OUTER_BOUND('',#602,.T.);
#327=FACE_OUTER_BOUND('',#603,.T.);
#328=FACE_OUTER_BOUND('',#604,.T.);
#329=FACE_OUTER_BOUND('',#605,.T.);
#330=FACE_OUTER_BOUND('',#606,.T.);
#331=FACE_OUTER_BOUND('',#607,.T.);
#332=FACE_OUTER_BOUND('',#608,.T.);
#333=FACE_OUTER_BOUND('',#609,.T.);
#334=FACE_OUTER_BOUND('',#610,.T.);
#335=FACE_OUTER_BOUND('',#611,.T.);
#336=FACE_OUTER_BOUND('',#612,.T.);
#337=FACE_OUTER_BOUND('',#613,.T.);
#338=FACE_OUTER_BOUND('',#614,.T.);
#339=FACE_OUTER_BOUND('',#615,.T.);
#340=FACE_OUTER_BOUND('',#616,.T.);
#341=FACE_OUTER_BOUND('',#617,.T.);
#342=FACE_OUTER_BOUND('',#618,.T.);
#343=FACE_OUTER_BOUND('',#619,.T.);
#344=FACE_OUTER_BOUND('',#620,.T.);
#345=FACE_OUTER_BOUND('',#621,.T.);
#346=FACE_OUTER_BOUND('',#622,.T.);
#347=FACE_OUTER_BOUND('',#623,.T.);
#348=FACE_OUTER_BOUND('',#624,.T.);
#349=FACE_OUTER_BOUND('',#625,.T.);
#350=FACE_OUTER_BOUND('',#626,.T.);
#351=FACE_OUTER_BOUND('',#627,.T.);
#352=FACE_OUTER_BOUND('',#628,.T.);
#353=FACE_OUTER_BOUND('',#629,.T.);
#354=FACE_OUTER_BOUND('',#630,.T.);
#355=FACE_OUTER_BOUND('',#631,.T.);
#356=FACE_OUTER_BOUND('',#632,.T.);
#357=FACE_OUTER_BOUND('',#633,.T.);
#358=FACE_OUTER_BOUND('',#634,.T.);
#359=FACE_OUTER_BOUND('',#635,.T.);
#360=FACE_OUTER_BOUND('',#636,.T.);
#361=FACE_OUTER_BOUND('',#637,.T.);
#362=FACE_OUTER_BOUND('',#638,.T.);
#363=FACE_OUTER_BOUND('',#639,.T.);
#364=FACE_OUTER_BOUND('',#640,.T.);
#365=FACE_OUTER_BOUND('',#641,.T.);
#366=FACE_OUTER_BOUND('',#642,.T.);
#367=FACE_OUTER_BOUND('',#643,.T.);
#368=FACE_OUTER_BOUND('',#644,.T.);
#369=FACE_OUTER_BOUND('',#645,.T.);
#370=FACE_OUTER_BOUND('',#646,.T.);
#371=FACE_OUTER_BOUND('',#647,.T.);
#372=FACE_OUTER_BOUND('',#648,.T.);
#373=FACE_OUTER_BOUND('',#649,.T.);
#374=FACE_OUTER_BOUND('',#650,.T.);
#375=FACE_OUTER_BOUND('',#651,.T.);
#376=FACE_OUTER_BOUND('',#652,.T.);
#377=FACE_OUTER_BOUND('',#653,.T.);
#378=FACE_OUTER_BOUND('',#654,.T.);
#379=FACE_OUTER_BOUND('',#655,.T.);
#380=FACE_OUTER_BOUND('',#656,.T.);
#381=FACE_OUTER_BOUND('',#657,.T.);
#382=FACE_OUTER_BOUND('',#658,.T.);
#383=FACE_OUTER_BOUND('',#659,.T.);
#384=FACE_OUTER_BOUND('',#660,.T.);
#385=FACE_OUTER_BOUND('',#661,.T.);
#386=FACE_OUTER_BOUND('',#662,.T.);
#387=FACE_OUTER_BOUND('',#663,.T.);
#388=FACE_OUTER_BOUND('',#664,.T.);
#389=FACE_OUTER_BOUND('',#665,.T.);
#390=FACE_OUTER_BOUND('',#666,.T.);
#391=FACE_OUTER_BOUND('',#667,.T.);
#392=FACE_OUTER_BOUND('',#668,.T.);
#393=FACE_OUTER_BOUND('',#669,.T.);
#394=FACE_OUTER_BOUND('',#670,.T.);
#395=FACE_OUTER_BOUND('',#671,.T.);
#396=FACE_OUTER_BOUND('',#672,.T.);
#397=FACE_OUTER_BOUND('',#673,.T.);
#398=FACE_OUTER_BOUND('',#674,.T.);
#399=FACE_OUTER_BOUND('',#675,.T.);
#400=FACE_OUTER_BOUND('',#676,.T.);
#401=FACE_OUTER_BOUND('',#677,.T.);
#402=FACE_OUTER_BOUND('',#678,.T.);
#403=FACE_OUTER_BOUND('',#679,.T.);
#404=FACE_OUTER_BOUND('',#680,.T.);
#405=FACE_OUTER_BOUND('',#681,.T.);
#406=FACE_OUTER_BOUND('',#682,.T.);
#407=FACE_OUTER_BOUND('',#683,.T.);
#408=FACE_OUTER_BOUND('',#684,.T.);
#409=FACE_OUTER_BOUND('',#685,.T.);
#410=FACE_OUTER_BOUND('',#686,.T.);
#411=FACE_OUTER_BOUND('',#687,.T.);
#412=FACE_OUTER_BOUND('',#688,.T.);
#413=FACE_OUTER_BOUND('',#689,.T.);
#414=FACE_OUTER_BOUND('',#690,.T.);
#415=FACE_OUTER_BOUND('',#691,.T.);
#416=FACE_OUTER_BOUND('',#692,.T.);
#417=FACE_OUTER_BOUND('',#693,.T.);
#418=FACE_OUTER_BOUND('',#694,.T.);
#419=FACE_OUTER_BOUND('',#695,.T.);
#420=FACE_OUTER_BOUND('',#696,.T.);
#421=FACE_OUTER_BOUND('',#697,.T.);
#422=FACE_OUTER_BOUND('',#698,.T.);
#423=FACE_OUTER_BOUND('',#699,.T.);
#424=FACE_OUTER_BOUND('',#700,.T.);
#425=FACE_OUTER_BOUND('',#701,.T.);
#426=FACE_OUTER_BOUND('',#702,.T.);
#427=FACE_OUTER_BOUND('',#703,.T.);
#428=FACE_OUTER_BOUND('',#704,.T.);
#429=FACE_OUTER_BOUND('',#705,.T.);
#430=FACE_OUTER_BOUND('',#706,.T.);
#431=FACE_OUTER_BOUND('',#707,.T.);
#432=FACE_OUTER_BOUND('',#708,.T.);
#433=FACE_OUTER_BOUND('',#709,.T.);
#434=FACE_OUTER_BOUND('',#710,.T.);
#435=FACE_OUTER_BOUND('',#711,.T.);
#436=FACE_OUTER_BOUND('',#712,.T.);
#437=FACE_OUTER_BOUND('',#713,.T.);
#438=FACE_OUTER_BOUND('',#714,.T.);
#439=FACE_OUTER_BOUND('',#715,.T.);
#440=FACE_OUTER_BOUND('',#716,.T.);
#441=FACE_OUTER_BOUND('',#717,.T.);
#442=FACE_OUTER_BOUND('',#718,.T.);
#443=FACE_OUTER_BOUND('',#719,.T.);
#444=FACE_OUTER_BOUND('',#720,.T.);
#445=FACE_OUTER_BOUND('',#721,.T.);
#446=FACE_OUTER_BOUND('',#722,.T.);
#447=FACE_OUTER_BOUND('',#723,.T.);
#448=FACE_OUTER_BOUND('',#724,.T.);
#449=FACE_OUTER_BOUND('',#725,.T.);
#450=FACE_OUTER_BOUND('',#726,.T.);
#451=FACE_OUTER_BOUND('',#727,.T.);
#452=FACE_OUTER_BOUND('',#728,.T.);
#453=FACE_OUTER_BOUND('',#729,.T.);
#454=FACE_OUTER_BOUND('',#730,.T.);
#455=FACE_OUTER_BOUND('',#731,.T.);
#456=FACE_OUTER_BOUND('',#732,.T.);
#457=FACE_OUTER_BOUND('',#733,.T.);
#458=FACE_OUTER_BOUND('',#734,.T.);
#459=FACE_OUTER_BOUND('',#735,.T.);
#460=FACE_OUTER_BOUND('',#737,.T.);
#461=FACE_OUTER_BOUND('',#739,.T.);
#462=FACE_OUTER_BOUND('',#740,.T.);
#463=FACE_OUTER_BOUND('',#741,.T.);
#464=FACE_OUTER_BOUND('',#742,.T.);
#465=FACE_OUTER_BOUND('',#743,.T.);
#466=FACE_OUTER_BOUND('',#744,.T.);
#467=FACE_OUTER_BOUND('',#745,.T.);
#468=FACE_OUTER_BOUND('',#746,.T.);
#469=FACE_OUTER_BOUND('',#747,.T.);
#470=FACE_OUTER_BOUND('',#748,.T.);
#471=FACE_OUTER_BOUND('',#749,.T.);
#472=FACE_OUTER_BOUND('',#750,.T.);
#473=FACE_OUTER_BOUND('',#751,.T.);
#474=FACE_OUTER_BOUND('',#752,.T.);
#475=FACE_OUTER_BOUND('',#753,.T.);
#476=FACE_OUTER_BOUND('',#754,.T.);
#477=FACE_OUTER_BOUND('',#755,.T.);
#478=FACE_OUTER_BOUND('',#756,.T.);
#479=FACE_OUTER_BOUND('',#757,.T.);
#480=FACE_OUTER_BOUND('',#758,.T.);
#481=FACE_OUTER_BOUND('',#759,.T.);
#482=FACE_OUTER_BOUND('',#760,.T.);
#483=FACE_OUTER_BOUND('',#761,.T.);
#484=FACE_OUTER_BOUND('',#762,.T.);
#485=FACE_OUTER_BOUND('',#763,.T.);
#486=FACE_OUTER_BOUND('',#764,.T.);
#487=FACE_OUTER_BOUND('',#765,.T.);
#488=FACE_OUTER_BOUND('',#766,.T.);
#489=FACE_OUTER_BOUND('',#767,.T.);
#490=FACE_OUTER_BOUND('',#768,.T.);
#491=FACE_OUTER_BOUND('',#769,.T.);
#492=FACE_OUTER_BOUND('',#770,.T.);
#493=FACE_OUTER_BOUND('',#771,.T.);
#494=FACE_OUTER_BOUND('',#772,.T.);
#495=FACE_OUTER_BOUND('',#773,.T.);
#496=FACE_OUTER_BOUND('',#774,.T.);
#497=FACE_OUTER_BOUND('',#775,.T.);
#498=FACE_OUTER_BOUND('',#776,.T.);
#499=FACE_OUTER_BOUND('',#777,.T.);
#500=FACE_OUTER_BOUND('',#778,.T.);
#501=FACE_OUTER_BOUND('',#779,.T.);
#502=FACE_OUTER_BOUND('',#780,.T.);
#503=FACE_OUTER_BOUND('',#781,.T.);
#504=FACE_OUTER_BOUND('',#782,.T.);
#505=FACE_OUTER_BOUND('',#784,.T.);
#506=FACE_OUTER_BOUND('',#785,.T.);
#507=FACE_OUTER_BOUND('',#786,.T.);
#508=FACE_OUTER_BOUND('',#787,.T.);
#509=FACE_OUTER_BOUND('',#788,.T.);
#510=FACE_OUTER_BOUND('',#789,.T.);
#511=FACE_OUTER_BOUND('',#790,.T.);
#512=FACE_OUTER_BOUND('',#791,.T.);
#513=FACE_OUTER_BOUND('',#792,.T.);
#514=FACE_OUTER_BOUND('',#793,.T.);
#515=FACE_OUTER_BOUND('',#794,.T.);
#516=FACE_OUTER_BOUND('',#795,.T.);
#517=FACE_OUTER_BOUND('',#796,.T.);
#518=FACE_OUTER_BOUND('',#797,.T.);
#519=FACE_OUTER_BOUND('',#798,.T.);
#520=FACE_OUTER_BOUND('',#799,.T.);
#521=FACE_OUTER_BOUND('',#800,.T.);
#522=FACE_OUTER_BOUND('',#801,.T.);
#523=FACE_OUTER_BOUND('',#802,.T.);
#524=FACE_OUTER_BOUND('',#804,.T.);
#525=FACE_OUTER_BOUND('',#805,.T.);
#526=FACE_OUTER_BOUND('',#806,.T.);
#527=FACE_OUTER_BOUND('',#807,.T.);
#528=FACE_OUTER_BOUND('',#809,.T.);
#529=FACE_OUTER_BOUND('',#810,.T.);
#530=FACE_OUTER_BOUND('',#811,.T.);
#531=FACE_OUTER_BOUND('',#812,.T.);
#532=FACE_OUTER_BOUND('',#813,.T.);
#533=FACE_OUTER_BOUND('',#815,.T.);
#534=FACE_OUTER_BOUND('',#816,.T.);
#535=FACE_OUTER_BOUND('',#817,.T.);
#536=FACE_OUTER_BOUND('',#818,.T.);
#537=FACE_OUTER_BOUND('',#820,.T.);
#538=FACE_OUTER_BOUND('',#821,.T.);
#539=FACE_OUTER_BOUND('',#823,.T.);
#540=FACE_OUTER_BOUND('',#824,.T.);
#541=FACE_OUTER_BOUND('',#825,.T.);
#542=FACE_OUTER_BOUND('',#826,.T.);
#543=FACE_OUTER_BOUND('',#828,.T.);
#544=FACE_OUTER_BOUND('',#829,.T.);
#545=FACE_OUTER_BOUND('',#830,.T.);
#546=FACE_OUTER_BOUND('',#832,.T.);
#547=FACE_OUTER_BOUND('',#833,.T.);
#548=FACE_OUTER_BOUND('',#835,.T.);
#549=FACE_OUTER_BOUND('',#836,.T.);
#550=FACE_OUTER_BOUND('',#838,.T.);
#551=FACE_OUTER_BOUND('',#839,.T.);
#552=FACE_OUTER_BOUND('',#841,.T.);
#553=FACE_OUTER_BOUND('',#842,.T.);
#554=FACE_OUTER_BOUND('',#843,.T.);
#555=FACE_OUTER_BOUND('',#844,.T.);
#556=FACE_OUTER_BOUND('',#845,.T.);
#557=FACE_OUTER_BOUND('',#846,.T.);
#558=FACE_OUTER_BOUND('',#847,.T.);
#559=FACE_OUTER_BOUND('',#848,.T.);
#560=FACE_OUTER_BOUND('',#850,.T.);
#561=FACE_OUTER_BOUND('',#851,.T.);
#562=FACE_OUTER_BOUND('',#852,.T.);
#563=FACE_OUTER_BOUND('',#853,.T.);
#564=FACE_OUTER_BOUND('',#854,.T.);
#565=FACE_OUTER_BOUND('',#855,.T.);
#566=FACE_OUTER_BOUND('',#856,.T.);
#567=FACE_OUTER_BOUND('',#857,.T.);
#568=FACE_OUTER_BOUND('',#858,.T.);
#569=FACE_OUTER_BOUND('',#859,.T.);
#570=FACE_OUTER_BOUND('',#860,.T.);
#571=FACE_OUTER_BOUND('',#861,.T.);
#572=FACE_OUTER_BOUND('',#862,.T.);
#573=FACE_OUTER_BOUND('',#863,.T.);
#574=FACE_OUTER_BOUND('',#864,.T.);
#575=FACE_OUTER_BOUND('',#865,.T.);
#576=FACE_OUTER_BOUND('',#866,.T.);
#577=FACE_OUTER_BOUND('',#867,.T.);
#578=FACE_OUTER_BOUND('',#868,.T.);
#579=FACE_OUTER_BOUND('',#869,.T.);
#580=FACE_OUTER_BOUND('',#870,.T.);
#581=FACE_OUTER_BOUND('',#872,.T.);
#582=FACE_OUTER_BOUND('',#873,.T.);
#583=FACE_OUTER_BOUND('',#874,.T.);
#584=FACE_OUTER_BOUND('',#875,.T.);
#585=FACE_OUTER_BOUND('',#876,.T.);
#586=FACE_OUTER_BOUND('',#877,.T.);
#587=FACE_OUTER_BOUND('',#878,.T.);
#588=FACE_OUTER_BOUND('',#879,.T.);
#589=FACE_OUTER_BOUND('',#880,.T.);
#590=FACE_OUTER_BOUND('',#881,.T.);
#591=FACE_OUTER_BOUND('',#882,.T.);
#592=FACE_OUTER_BOUND('',#883,.T.);
#593=FACE_OUTER_BOUND('',#884,.T.);
#594=FACE_OUTER_BOUND('',#885,.T.);
#595=FACE_OUTER_BOUND('',#888,.T.);
#596=FACE_OUTER_BOUND('',#890,.T.);
#597=FACE_OUTER_BOUND('',#891,.T.);
#598=FACE_OUTER_BOUND('',#893,.T.);
#599=FACE_OUTER_BOUND('',#894,.T.);
#600=FACE_OUTER_BOUND('',#896,.T.);
#601=EDGE_LOOP('',(#3027,#3028,#3029,#3030));
#602=EDGE_LOOP('',(#3031,#3032,#3033,#3034));
#603=EDGE_LOOP('',(#3035,#3036,#3037,#3038));
#604=EDGE_LOOP('',(#3039,#3040,#3041,#3042));
#605=EDGE_LOOP('',(#3043,#3044,#3045,#3046));
#606=EDGE_LOOP('',(#3047,#3048,#3049,#3050));
#607=EDGE_LOOP('',(#3051,#3052,#3053,#3054));
#608=EDGE_LOOP('',(#3055,#3056,#3057,#3058));
#609=EDGE_LOOP('',(#3059,#3060,#3061,#3062));
#610=EDGE_LOOP('',(#3063,#3064,#3065,#3066));
#611=EDGE_LOOP('',(#3067,#3068,#3069,#3070));
#612=EDGE_LOOP('',(#3071,#3072,#3073,#3074));
#613=EDGE_LOOP('',(#3075,#3076,#3077,#3078));
#614=EDGE_LOOP('',(#3079,#3080,#3081,#3082));
#615=EDGE_LOOP('',(#3083,#3084,#3085,#3086));
#616=EDGE_LOOP('',(#3087,#3088,#3089,#3090));
#617=EDGE_LOOP('',(#3091,#3092,#3093,#3094));
#618=EDGE_LOOP('',(#3095,#3096,#3097,#3098));
#619=EDGE_LOOP('',(#3099,#3100,#3101,#3102));
#620=EDGE_LOOP('',(#3103,#3104,#3105,#3106));
#621=EDGE_LOOP('',(#3107,#3108,#3109,#3110));
#622=EDGE_LOOP('',(#3111,#3112,#3113,#3114));
#623=EDGE_LOOP('',(#3115,#3116,#3117,#3118));
#624=EDGE_LOOP('',(#3119,#3120,#3121,#3122));
#625=EDGE_LOOP('',(#3123,#3124,#3125,#3126));
#626=EDGE_LOOP('',(#3127,#3128,#3129,#3130));
#627=EDGE_LOOP('',(#3131,#3132,#3133,#3134));
#628=EDGE_LOOP('',(#3135,#3136,#3137,#3138));
#629=EDGE_LOOP('',(#3139,#3140,#3141,#3142));
#630=EDGE_LOOP('',(#3143,#3144,#3145,#3146));
#631=EDGE_LOOP('',(#3147,#3148,#3149,#3150));
#632=EDGE_LOOP('',(#3151,#3152,#3153,#3154));
#633=EDGE_LOOP('',(#3155,#3156,#3157,#3158));
#634=EDGE_LOOP('',(#3159,#3160,#3161,#3162));
#635=EDGE_LOOP('',(#3163,#3164,#3165,#3166));
#636=EDGE_LOOP('',(#3167,#3168,#3169,#3170));
#637=EDGE_LOOP('',(#3171,#3172,#3173,#3174));
#638=EDGE_LOOP('',(#3175,#3176,#3177,#3178));
#639=EDGE_LOOP('',(#3179,#3180,#3181,#3182));
#640=EDGE_LOOP('',(#3183,#3184,#3185,#3186));
#641=EDGE_LOOP('',(#3187,#3188,#3189,#3190));
#642=EDGE_LOOP('',(#3191,#3192,#3193,#3194));
#643=EDGE_LOOP('',(#3195,#3196,#3197,#3198));
#644=EDGE_LOOP('',(#3199,#3200,#3201,#3202));
#645=EDGE_LOOP('',(#3203,#3204,#3205,#3206));
#646=EDGE_LOOP('',(#3207,#3208,#3209,#3210));
#647=EDGE_LOOP('',(#3211,#3212,#3213,#3214));
#648=EDGE_LOOP('',(#3215,#3216,#3217,#3218));
#649=EDGE_LOOP('',(#3219,#3220,#3221,#3222));
#650=EDGE_LOOP('',(#3223,#3224,#3225,#3226));
#651=EDGE_LOOP('',(#3227,#3228,#3229,#3230));
#652=EDGE_LOOP('',(#3231,#3232,#3233,#3234));
#653=EDGE_LOOP('',(#3235,#3236,#3237,#3238));
#654=EDGE_LOOP('',(#3239,#3240,#3241,#3242));
#655=EDGE_LOOP('',(#3243,#3244,#3245,#3246));
#656=EDGE_LOOP('',(#3247,#3248,#3249,#3250));
#657=EDGE_LOOP('',(#3251,#3252,#3253,#3254));
#658=EDGE_LOOP('',(#3255,#3256,#3257,#3258));
#659=EDGE_LOOP('',(#3259,#3260,#3261,#3262));
#660=EDGE_LOOP('',(#3263,#3264,#3265,#3266));
#661=EDGE_LOOP('',(#3267,#3268,#3269,#3270));
#662=EDGE_LOOP('',(#3271,#3272,#3273,#3274));
#663=EDGE_LOOP('',(#3275,#3276,#3277,#3278));
#664=EDGE_LOOP('',(#3279,#3280,#3281,#3282));
#665=EDGE_LOOP('',(#3283,#3284,#3285,#3286));
#666=EDGE_LOOP('',(#3287,#3288,#3289,#3290));
#667=EDGE_LOOP('',(#3291,#3292,#3293,#3294));
#668=EDGE_LOOP('',(#3295,#3296,#3297,#3298));
#669=EDGE_LOOP('',(#3299,#3300,#3301,#3302));
#670=EDGE_LOOP('',(#3303,#3304,#3305,#3306));
#671=EDGE_LOOP('',(#3307,#3308,#3309,#3310));
#672=EDGE_LOOP('',(#3311,#3312,#3313,#3314));
#673=EDGE_LOOP('',(#3315,#3316,#3317,#3318));
#674=EDGE_LOOP('',(#3319,#3320,#3321,#3322));
#675=EDGE_LOOP('',(#3323,#3324,#3325,#3326));
#676=EDGE_LOOP('',(#3327,#3328,#3329,#3330));
#677=EDGE_LOOP('',(#3331,#3332,#3333,#3334));
#678=EDGE_LOOP('',(#3335,#3336,#3337,#3338));
#679=EDGE_LOOP('',(#3339,#3340,#3341,#3342));
#680=EDGE_LOOP('',(#3343,#3344,#3345,#3346));
#681=EDGE_LOOP('',(#3347,#3348,#3349,#3350));
#682=EDGE_LOOP('',(#3351,#3352,#3353,#3354));
#683=EDGE_LOOP('',(#3355,#3356,#3357,#3358));
#684=EDGE_LOOP('',(#3359,#3360,#3361,#3362));
#685=EDGE_LOOP('',(#3363,#3364,#3365,#3366));
#686=EDGE_LOOP('',(#3367,#3368,#3369,#3370));
#687=EDGE_LOOP('',(#3371,#3372,#3373,#3374));
#688=EDGE_LOOP('',(#3375,#3376,#3377,#3378));
#689=EDGE_LOOP('',(#3379,#3380,#3381,#3382));
#690=EDGE_LOOP('',(#3383,#3384,#3385,#3386));
#691=EDGE_LOOP('',(#3387,#3388,#3389,#3390));
#692=EDGE_LOOP('',(#3391,#3392,#3393,#3394));
#693=EDGE_LOOP('',(#3395,#3396,#3397,#3398));
#694=EDGE_LOOP('',(#3399,#3400,#3401,#3402));
#695=EDGE_LOOP('',(#3403,#3404,#3405,#3406));
#696=EDGE_LOOP('',(#3407,#3408,#3409,#3410));
#697=EDGE_LOOP('',(#3411,#3412,#3413,#3414));
#698=EDGE_LOOP('',(#3415,#3416,#3417,#3418));
#699=EDGE_LOOP('',(#3419,#3420,#3421,#3422));
#700=EDGE_LOOP('',(#3423,#3424,#3425,#3426));
#701=EDGE_LOOP('',(#3427,#3428,#3429,#3430));
#702=EDGE_LOOP('',(#3431,#3432,#3433,#3434));
#703=EDGE_LOOP('',(#3435,#3436,#3437,#3438));
#704=EDGE_LOOP('',(#3439,#3440,#3441,#3442));
#705=EDGE_LOOP('',(#3443,#3444,#3445,#3446));
#706=EDGE_LOOP('',(#3447,#3448,#3449,#3450));
#707=EDGE_LOOP('',(#3451,#3452,#3453,#3454));
#708=EDGE_LOOP('',(#3455,#3456,#3457,#3458));
#709=EDGE_LOOP('',(#3459,#3460,#3461,#3462));
#710=EDGE_LOOP('',(#3463,#3464,#3465,#3466));
#711=EDGE_LOOP('',(#3467,#3468,#3469,#3470));
#712=EDGE_LOOP('',(#3471,#3472,#3473,#3474));
#713=EDGE_LOOP('',(#3475,#3476,#3477,#3478));
#714=EDGE_LOOP('',(#3479,#3480,#3481,#3482));
#715=EDGE_LOOP('',(#3483,#3484,#3485,#3486));
#716=EDGE_LOOP('',(#3487,#3488,#3489,#3490));
#717=EDGE_LOOP('',(#3491,#3492,#3493,#3494));
#718=EDGE_LOOP('',(#3495,#3496,#3497,#3498));
#719=EDGE_LOOP('',(#3499,#3500,#3501,#3502));
#720=EDGE_LOOP('',(#3503,#3504,#3505,#3506));
#721=EDGE_LOOP('',(#3507,#3508,#3509,#3510));
#722=EDGE_LOOP('',(#3511,#3512,#3513,#3514));
#723=EDGE_LOOP('',(#3515,#3516,#3517,#3518));
#724=EDGE_LOOP('',(#3519,#3520,#3521,#3522));
#725=EDGE_LOOP('',(#3523,#3524,#3525,#3526));
#726=EDGE_LOOP('',(#3527,#3528,#3529,#3530));
#727=EDGE_LOOP('',(#3531,#3532,#3533,#3534));
#728=EDGE_LOOP('',(#3535,#3536,#3537,#3538));
#729=EDGE_LOOP('',(#3539,#3540,#3541,#3542));
#730=EDGE_LOOP('',(#3543,#3544,#3545,#3546));
#731=EDGE_LOOP('',(#3547,#3548,#3549,#3550));
#732=EDGE_LOOP('',(#3551,#3552,#3553,#3554));
#733=EDGE_LOOP('',(#3555,#3556,#3557,#3558));
#734=EDGE_LOOP('',(#3559,#3560,#3561,#3562));
#735=EDGE_LOOP('',(#3563,#3564,#3565,#3566,#3567,#3568,#3569,#3570,#3571,
#3572,#3573,#3574,#3575,#3576,#3577,#3578,#3579,#3580,#3581,#3582,#3583,
#3584,#3585,#3586,#3587,#3588,#3589,#3590,#3591,#3592,#3593,#3594,#3595,
#3596,#3597,#3598,#3599,#3600,#3601,#3602,#3603,#3604,#3605,#3606,#3607,
#3608,#3609,#3610,#3611,#3612,#3613,#3614,#3615,#3616,#3617,#3618,#3619,
#3620,#3621,#3622,#3623,#3624,#3625,#3626,#3627,#3628,#3629,#3630,#3631,
#3632,#3633,#3634,#3635,#3636,#3637,#3638,#3639,#3640,#3641,#3642,#3643,
#3644,#3645,#3646,#3647,#3648,#3649,#3650,#3651,#3652,#3653,#3654,#3655,
#3656,#3657,#3658,#3659,#3660,#3661,#3662,#3663,#3664,#3665,#3666,#3667,
#3668,#3669,#3670,#3671,#3672,#3673,#3674,#3675,#3676,#3677,#3678,#3679,
#3680,#3681,#3682,#3683,#3684,#3685,#3686,#3687,#3688,#3689,#3690,#3691,
#3692,#3693,#3694,#3695,#3696,#3697,#3698,#3699,#3700,#3701,#3702,#3703,
#3704,#3705,#3706,#3707,#3708,#3709,#3710,#3711,#3712,#3713,#3714,#3715,
#3716,#3717,#3718,#3719,#3720,#3721,#3722));
#736=EDGE_LOOP('',(#3723));
#737=EDGE_LOOP('',(#3724,#3725,#3726,#3727,#3728,#3729,#3730,#3731,#3732,
#3733,#3734,#3735,#3736,#3737,#3738,#3739,#3740,#3741,#3742,#3743,#3744,
#3745,#3746,#3747,#3748,#3749,#3750,#3751,#3752,#3753,#3754,#3755,#3756,
#3757,#3758,#3759,#3760,#3761,#3762,#3763,#3764,#3765,#3766,#3767,#3768,
#3769,#3770,#3771,#3772,#3773,#3774,#3775,#3776,#3777,#3778,#3779,#3780,
#3781,#3782,#3783,#3784,#3785,#3786,#3787,#3788,#3789,#3790,#3791,#3792,
#3793,#3794,#3795,#3796,#3797,#3798,#3799,#3800,#3801,#3802,#3803,#3804,
#3805,#3806,#3807,#3808,#3809,#3810,#3811,#3812,#3813,#3814,#3815,#3816,
#3817,#3818,#3819,#3820,#3821,#3822,#3823,#3824,#3825,#3826,#3827,#3828,
#3829,#3830,#3831,#3832,#3833,#3834,#3835,#3836,#3837,#3838,#3839,#3840,
#3841,#3842,#3843,#3844,#3845,#3846,#3847,#3848,#3849,#3850,#3851,#3852,
#3853,#3854,#3855,#3856,#3857,#3858,#3859,#3860,#3861,#3862,#3863,#3864,
#3865,#3866,#3867,#3868,#3869,#3870,#3871,#3872,#3873,#3874,#3875,#3876,
#3877,#3878,#3879,#3880,#3881,#3882,#3883));
#738=EDGE_LOOP('',(#3884));
#739=EDGE_LOOP('',(#3885,#3886,#3887,#3888));
#740=EDGE_LOOP('',(#3889,#3890,#3891,#3892));
#741=EDGE_LOOP('',(#3893,#3894,#3895,#3896));
#742=EDGE_LOOP('',(#3897,#3898,#3899,#3900));
#743=EDGE_LOOP('',(#3901,#3902,#3903,#3904));
#744=EDGE_LOOP('',(#3905,#3906,#3907,#3908));
#745=EDGE_LOOP('',(#3909,#3910,#3911,#3912));
#746=EDGE_LOOP('',(#3913,#3914,#3915,#3916));
#747=EDGE_LOOP('',(#3917,#3918,#3919,#3920));
#748=EDGE_LOOP('',(#3921,#3922,#3923,#3924));
#749=EDGE_LOOP('',(#3925,#3926,#3927,#3928));
#750=EDGE_LOOP('',(#3929,#3930,#3931,#3932));
#751=EDGE_LOOP('',(#3933,#3934,#3935,#3936));
#752=EDGE_LOOP('',(#3937,#3938,#3939,#3940));
#753=EDGE_LOOP('',(#3941,#3942,#3943,#3944));
#754=EDGE_LOOP('',(#3945,#3946,#3947,#3948));
#755=EDGE_LOOP('',(#3949,#3950,#3951,#3952));
#756=EDGE_LOOP('',(#3953,#3954,#3955,#3956));
#757=EDGE_LOOP('',(#3957,#3958,#3959,#3960));
#758=EDGE_LOOP('',(#3961,#3962,#3963,#3964));
#759=EDGE_LOOP('',(#3965,#3966,#3967,#3968));
#760=EDGE_LOOP('',(#3969,#3970,#3971,#3972));
#761=EDGE_LOOP('',(#3973,#3974,#3975,#3976));
#762=EDGE_LOOP('',(#3977,#3978,#3979,#3980));
#763=EDGE_LOOP('',(#3981,#3982,#3983,#3984));
#764=EDGE_LOOP('',(#3985,#3986,#3987,#3988));
#765=EDGE_LOOP('',(#3989,#3990,#3991,#3992));
#766=EDGE_LOOP('',(#3993,#3994,#3995,#3996));
#767=EDGE_LOOP('',(#3997,#3998,#3999,#4000));
#768=EDGE_LOOP('',(#4001,#4002,#4003,#4004));
#769=EDGE_LOOP('',(#4005,#4006,#4007,#4008));
#770=EDGE_LOOP('',(#4009,#4010,#4011));
#771=EDGE_LOOP('',(#4012,#4013,#4014));
#772=EDGE_LOOP('',(#4015,#4016,#4017));
#773=EDGE_LOOP('',(#4018,#4019,#4020));
#774=EDGE_LOOP('',(#4021,#4022,#4023));
#775=EDGE_LOOP('',(#4024,#4025,#4026));
#776=EDGE_LOOP('',(#4027,#4028,#4029,#4030));
#777=EDGE_LOOP('',(#4031,#4032,#4033,#4034));
#778=EDGE_LOOP('',(#4035,#4036,#4037,#4038));
#779=EDGE_LOOP('',(#4039,#4040,#4041,#4042));
#780=EDGE_LOOP('',(#4043,#4044,#4045,#4046));
#781=EDGE_LOOP('',(#4047,#4048,#4049,#4050));
#782=EDGE_LOOP('',(#4051));
#783=EDGE_LOOP('',(#4052,#4053,#4054,#4055,#4056,#4057));
#784=EDGE_LOOP('',(#4058,#4059,#4060,#4061));
#785=EDGE_LOOP('',(#4062));
#786=EDGE_LOOP('',(#4063,#4064,#4065,#4066));
#787=EDGE_LOOP('',(#4067,#4068,#4069,#4070));
#788=EDGE_LOOP('',(#4071,#4072,#4073,#4074));
#789=EDGE_LOOP('',(#4075,#4076,#4077,#4078));
#790=EDGE_LOOP('',(#4079,#4080,#4081));
#791=EDGE_LOOP('',(#4082,#4083,#4084));
#792=EDGE_LOOP('',(#4085,#4086,#4087));
#793=EDGE_LOOP('',(#4088,#4089,#4090));
#794=EDGE_LOOP('',(#4091,#4092,#4093));
#795=EDGE_LOOP('',(#4094,#4095,#4096));
#796=EDGE_LOOP('',(#4097,#4098,#4099,#4100));
#797=EDGE_LOOP('',(#4101,#4102,#4103,#4104));
#798=EDGE_LOOP('',(#4105,#4106,#4107,#4108));
#799=EDGE_LOOP('',(#4109,#4110,#4111,#4112));
#800=EDGE_LOOP('',(#4113,#4114,#4115,#4116));
#801=EDGE_LOOP('',(#4117,#4118,#4119,#4120));
#802=EDGE_LOOP('',(#4121));
#803=EDGE_LOOP('',(#4122,#4123,#4124,#4125,#4126,#4127));
#804=EDGE_LOOP('',(#4128,#4129,#4130,#4131));
#805=EDGE_LOOP('',(#4132));
#806=EDGE_LOOP('',(#4133,#4134,#4135,#4136));
#807=EDGE_LOOP('',(#4137));
#808=EDGE_LOOP('',(#4138));
#809=EDGE_LOOP('',(#4139,#4140,#4141,#4142));
#810=EDGE_LOOP('',(#4143,#4144,#4145,#4146));
#811=EDGE_LOOP('',(#4147));
#812=EDGE_LOOP('',(#4148,#4149,#4150,#4151));
#813=EDGE_LOOP('',(#4152));
#814=EDGE_LOOP('',(#4153));
#815=EDGE_LOOP('',(#4154));
#816=EDGE_LOOP('',(#4155,#4156,#4157,#4158));
#817=EDGE_LOOP('',(#4159,#4160,#4161,#4162));
#818=EDGE_LOOP('',(#4163));
#819=EDGE_LOOP('',(#4164));
#820=EDGE_LOOP('',(#4165,#4166,#4167,#4168));
#821=EDGE_LOOP('',(#4169));
#822=EDGE_LOOP('',(#4170));
#823=EDGE_LOOP('',(#4171,#4172,#4173,#4174));
#824=EDGE_LOOP('',(#4175,#4176,#4177,#4178));
#825=EDGE_LOOP('',(#4179,#4180,#4181,#4182));
#826=EDGE_LOOP('',(#4183));
#827=EDGE_LOOP('',(#4184));
#828=EDGE_LOOP('',(#4185,#4186,#4187,#4188));
#829=EDGE_LOOP('',(#4189,#4190,#4191,#4192));
#830=EDGE_LOOP('',(#4193));
#831=EDGE_LOOP('',(#4194));
#832=EDGE_LOOP('',(#4195,#4196,#4197,#4198));
#833=EDGE_LOOP('',(#4199));
#834=EDGE_LOOP('',(#4200));
#835=EDGE_LOOP('',(#4201,#4202,#4203,#4204));
#836=EDGE_LOOP('',(#4205));
#837=EDGE_LOOP('',(#4206));
#838=EDGE_LOOP('',(#4207,#4208,#4209,#4210));
#839=EDGE_LOOP('',(#4211));
#840=EDGE_LOOP('',(#4212));
#841=EDGE_LOOP('',(#4213,#4214,#4215,#4216));
#842=EDGE_LOOP('',(#4217,#4218,#4219,#4220));
#843=EDGE_LOOP('',(#4221,#4222,#4223));
#844=EDGE_LOOP('',(#4224,#4225,#4226,#4227));
#845=EDGE_LOOP('',(#4228,#4229,#4230));
#846=EDGE_LOOP('',(#4231,#4232,#4233,#4234,#4235,#4236));
#847=EDGE_LOOP('',(#4237,#4238,#4239,#4240));
#848=EDGE_LOOP('',(#4241,#4242,#4243,#4244,#4245,#4246));
#849=EDGE_LOOP('',(#4247));
#850=EDGE_LOOP('',(#4248,#4249,#4250,#4251));
#851=EDGE_LOOP('',(#4252,#4253,#4254,#4255,#4256,#4257));
#852=EDGE_LOOP('',(#4258,#4259,#4260,#4261));
#853=EDGE_LOOP('',(#4262,#4263,#4264,#4265));
#854=EDGE_LOOP('',(#4266,#4267,#4268,#4269));
#855=EDGE_LOOP('',(#4270,#4271,#4272,#4273));
#856=EDGE_LOOP('',(#4274,#4275,#4276,#4277));
#857=EDGE_LOOP('',(#4278,#4279,#4280,#4281));
#858=EDGE_LOOP('',(#4282,#4283,#4284,#4285));
#859=EDGE_LOOP('',(#4286,#4287,#4288,#4289));
#860=EDGE_LOOP('',(#4290,#4291,#4292,#4293));
#861=EDGE_LOOP('',(#4294,#4295,#4296,#4297));
#862=EDGE_LOOP('',(#4298,#4299,#4300,#4301));
#863=EDGE_LOOP('',(#4302,#4303,#4304,#4305));
#864=EDGE_LOOP('',(#4306,#4307,#4308,#4309));
#865=EDGE_LOOP('',(#4310,#4311,#4312));
#866=EDGE_LOOP('',(#4313,#4314,#4315,#4316));
#867=EDGE_LOOP('',(#4317,#4318,#4319));
#868=EDGE_LOOP('',(#4320,#4321,#4322,#4323,#4324,#4325));
#869=EDGE_LOOP('',(#4326,#4327,#4328,#4329));
#870=EDGE_LOOP('',(#4330,#4331,#4332,#4333,#4334,#4335));
#871=EDGE_LOOP('',(#4336));
#872=EDGE_LOOP('',(#4337,#4338,#4339,#4340));
#873=EDGE_LOOP('',(#4341,#4342,#4343,#4344,#4345,#4346));
#874=EDGE_LOOP('',(#4347,#4348,#4349,#4350));
#875=EDGE_LOOP('',(#4351,#4352,#4353,#4354));
#876=EDGE_LOOP('',(#4355,#4356,#4357,#4358));
#877=EDGE_LOOP('',(#4359,#4360,#4361,#4362));
#878=EDGE_LOOP('',(#4363,#4364,#4365,#4366));
#879=EDGE_LOOP('',(#4367,#4368,#4369,#4370));
#880=EDGE_LOOP('',(#4371,#4372,#4373,#4374));
#881=EDGE_LOOP('',(#4375,#4376,#4377,#4378));
#882=EDGE_LOOP('',(#4379,#4380,#4381,#4382));
#883=EDGE_LOOP('',(#4383,#4384,#4385,#4386));
#884=EDGE_LOOP('',(#4387));
#885=EDGE_LOOP('',(#4388,#4389,#4390,#4391,#4392,#4393,#4394,#4395,#4396,
#4397,#4398,#4399));
#886=EDGE_LOOP('',(#4400));
#887=EDGE_LOOP('',(#4401));
#888=EDGE_LOOP('',(#4402,#4403,#4404,#4405,#4406,#4407,#4408,#4409,#4410,
#4411,#4412,#4413));
#889=EDGE_LOOP('',(#4414));
#890=EDGE_LOOP('',(#4415,#4416,#4417,#4418));
#891=EDGE_LOOP('',(#4419));
#892=EDGE_LOOP('',(#4420));
#893=EDGE_LOOP('',(#4421,#4422,#4423,#4424));
#894=EDGE_LOOP('',(#4425));
#895=EDGE_LOOP('',(#4426));
#896=EDGE_LOOP('',(#4427,#4428,#4429,#4430));
#897=LINE('',#6823,#1253);
#898=LINE('',#6830,#1254);
#899=LINE('',#6833,#1255);
#900=LINE('',#6836,#1256);
#901=LINE('',#6838,#1257);
#902=LINE('',#6839,#1258);
#903=LINE('',#6845,#1259);
#904=LINE('',#6848,#1260);
#905=LINE('',#6851,#1261);
#906=LINE('',#6853,#1262);
#907=LINE('',#6854,#1263);
#908=LINE('',#6860,#1264);
#909=LINE('',#6863,#1265);
#910=LINE('',#6866,#1266);
#911=LINE('',#6868,#1267);
#912=LINE('',#6869,#1268);
#913=LINE('',#6875,#1269);
#914=LINE('',#6878,#1270);
#915=LINE('',#6881,#1271);
#916=LINE('',#6883,#1272);
#917=LINE('',#6884,#1273);
#918=LINE('',#6890,#1274);
#919=LINE('',#6893,#1275);
#920=LINE('',#6896,#1276);
#921=LINE('',#6898,#1277);
#922=LINE('',#6899,#1278);
#923=LINE('',#6905,#1279);
#924=LINE('',#6908,#1280);
#925=LINE('',#6911,#1281);
#926=LINE('',#6913,#1282);
#927=LINE('',#6914,#1283);
#928=LINE('',#6920,#1284);
#929=LINE('',#6923,#1285);
#930=LINE('',#6926,#1286);
#931=LINE('',#6928,#1287);
#932=LINE('',#6929,#1288);
#933=LINE('',#6935,#1289);
#934=LINE('',#6938,#1290);
#935=LINE('',#6941,#1291);
#936=LINE('',#6943,#1292);
#937=LINE('',#6944,#1293);
#938=LINE('',#6950,#1294);
#939=LINE('',#6953,#1295);
#940=LINE('',#6956,#1296);
#941=LINE('',#6958,#1297);
#942=LINE('',#6959,#1298);
#943=LINE('',#6965,#1299);
#944=LINE('',#6968,#1300);
#945=LINE('',#6971,#1301);
#946=LINE('',#6973,#1302);
#947=LINE('',#6974,#1303);
#948=LINE('',#6980,#1304);
#949=LINE('',#6983,#1305);
#950=LINE('',#6986,#1306);
#951=LINE('',#6988,#1307);
#952=LINE('',#6989,#1308);
#953=LINE('',#6995,#1309);
#954=LINE('',#6998,#1310);
#955=LINE('',#7001,#1311);
#956=LINE('',#7003,#1312);
#957=LINE('',#7004,#1313);
#958=LINE('',#7010,#1314);
#959=LINE('',#7013,#1315);
#960=LINE('',#7016,#1316);
#961=LINE('',#7018,#1317);
#962=LINE('',#7019,#1318);
#963=LINE('',#7025,#1319);
#964=LINE('',#7028,#1320);
#965=LINE('',#7031,#1321);
#966=LINE('',#7033,#1322);
#967=LINE('',#7034,#1323);
#968=LINE('',#7040,#1324);
#969=LINE('',#7043,#1325);
#970=LINE('',#7046,#1326);
#971=LINE('',#7048,#1327);
#972=LINE('',#7049,#1328);
#973=LINE('',#7055,#1329);
#974=LINE('',#7058,#1330);
#975=LINE('',#7061,#1331);
#976=LINE('',#7063,#1332);
#977=LINE('',#7064,#1333);
#978=LINE('',#7070,#1334);
#979=LINE('',#7073,#1335);
#980=LINE('',#7076,#1336);
#981=LINE('',#7078,#1337);
#982=LINE('',#7079,#1338);
#983=LINE('',#7085,#1339);
#984=LINE('',#7088,#1340);
#985=LINE('',#7091,#1341);
#986=LINE('',#7093,#1342);
#987=LINE('',#7094,#1343);
#988=LINE('',#7100,#1344);
#989=LINE('',#7103,#1345);
#990=LINE('',#7106,#1346);
#991=LINE('',#7108,#1347);
#992=LINE('',#7109,#1348);
#993=LINE('',#7115,#1349);
#994=LINE('',#7118,#1350);
#995=LINE('',#7121,#1351);
#996=LINE('',#7123,#1352);
#997=LINE('',#7124,#1353);
#998=LINE('',#7130,#1354);
#999=LINE('',#7133,#1355);
#1000=LINE('',#7136,#1356);
#1001=LINE('',#7138,#1357);
#1002=LINE('',#7139,#1358);
#1003=LINE('',#7145,#1359);
#1004=LINE('',#7148,#1360);
#1005=LINE('',#7151,#1361);
#1006=LINE('',#7153,#1362);
#1007=LINE('',#7154,#1363);
#1008=LINE('',#7160,#1364);
#1009=LINE('',#7163,#1365);
#1010=LINE('',#7166,#1366);
#1011=LINE('',#7168,#1367);
#1012=LINE('',#7169,#1368);
#1013=LINE('',#7175,#1369);
#1014=LINE('',#7178,#1370);
#1015=LINE('',#7181,#1371);
#1016=LINE('',#7183,#1372);
#1017=LINE('',#7184,#1373);
#1018=LINE('',#7190,#1374);
#1019=LINE('',#7193,#1375);
#1020=LINE('',#7196,#1376);
#1021=LINE('',#7198,#1377);
#1022=LINE('',#7199,#1378);
#1023=LINE('',#7205,#1379);
#1024=LINE('',#7208,#1380);
#1025=LINE('',#7211,#1381);
#1026=LINE('',#7213,#1382);
#1027=LINE('',#7214,#1383);
#1028=LINE('',#7220,#1384);
#1029=LINE('',#7223,#1385);
#1030=LINE('',#7226,#1386);
#1031=LINE('',#7228,#1387);
#1032=LINE('',#7229,#1388);
#1033=LINE('',#7235,#1389);
#1034=LINE('',#7238,#1390);
#1035=LINE('',#7241,#1391);
#1036=LINE('',#7243,#1392);
#1037=LINE('',#7244,#1393);
#1038=LINE('',#7250,#1394);
#1039=LINE('',#7253,#1395);
#1040=LINE('',#7256,#1396);
#1041=LINE('',#7258,#1397);
#1042=LINE('',#7259,#1398);
#1043=LINE('',#7265,#1399);
#1044=LINE('',#7268,#1400);
#1045=LINE('',#7271,#1401);
#1046=LINE('',#7273,#1402);
#1047=LINE('',#7274,#1403);
#1048=LINE('',#7280,#1404);
#1049=LINE('',#7283,#1405);
#1050=LINE('',#7286,#1406);
#1051=LINE('',#7288,#1407);
#1052=LINE('',#7289,#1408);
#1053=LINE('',#7295,#1409);
#1054=LINE('',#7298,#1410);
#1055=LINE('',#7301,#1411);
#1056=LINE('',#7303,#1412);
#1057=LINE('',#7304,#1413);
#1058=LINE('',#7310,#1414);
#1059=LINE('',#7313,#1415);
#1060=LINE('',#7316,#1416);
#1061=LINE('',#7318,#1417);
#1062=LINE('',#7319,#1418);
#1063=LINE('',#7325,#1419);
#1064=LINE('',#7328,#1420);
#1065=LINE('',#7331,#1421);
#1066=LINE('',#7333,#1422);
#1067=LINE('',#7334,#1423);
#1068=LINE('',#7340,#1424);
#1069=LINE('',#7343,#1425);
#1070=LINE('',#7346,#1426);
#1071=LINE('',#7348,#1427);
#1072=LINE('',#7349,#1428);
#1073=LINE('',#7355,#1429);
#1074=LINE('',#7358,#1430);
#1075=LINE('',#7361,#1431);
#1076=LINE('',#7363,#1432);
#1077=LINE('',#7364,#1433);
#1078=LINE('',#7370,#1434);
#1079=LINE('',#7373,#1435);
#1080=LINE('',#7376,#1436);
#1081=LINE('',#7378,#1437);
#1082=LINE('',#7379,#1438);
#1083=LINE('',#7385,#1439);
#1084=LINE('',#7388,#1440);
#1085=LINE('',#7391,#1441);
#1086=LINE('',#7393,#1442);
#1087=LINE('',#7394,#1443);
#1088=LINE('',#7688,#1444);
#1089=LINE('',#7694,#1445);
#1090=LINE('',#8282,#1446);
#1091=LINE('',#8288,#1447);
#1092=LINE('',#8882,#1448);
#1093=LINE('',#8888,#1449);
#1094=LINE('',#9476,#1450);
#1095=LINE('',#9482,#1451);
#1096=LINE('',#10070,#1452);
#1097=LINE('',#10076,#1453);
#1098=LINE('',#10664,#1454);
#1099=LINE('',#10670,#1455);
#1100=LINE('',#11258,#1456);
#1101=LINE('',#11264,#1457);
#1102=LINE('',#11852,#1458);
#1103=LINE('',#11858,#1459);
#1104=LINE('',#12446,#1460);
#1105=LINE('',#12452,#1461);
#1106=LINE('',#13040,#1462);
#1107=LINE('',#13046,#1463);
#1108=LINE('',#13634,#1464);
#1109=LINE('',#13640,#1465);
#1110=LINE('',#14228,#1466);
#1111=LINE('',#14234,#1467);
#1112=LINE('',#14822,#1468);
#1113=LINE('',#14828,#1469);
#1114=LINE('',#15416,#1470);
#1115=LINE('',#15422,#1471);
#1116=LINE('',#16010,#1472);
#1117=LINE('',#16016,#1473);
#1118=LINE('',#16604,#1474);
#1119=LINE('',#16610,#1475);
#1120=LINE('',#17213,#1476);
#1121=LINE('',#17219,#1477);
#1122=LINE('',#17807,#1478);
#1123=LINE('',#17813,#1479);
#1124=LINE('',#18401,#1480);
#1125=LINE('',#18407,#1481);
#1126=LINE('',#18725,#1482);
#1127=LINE('',#18879,#1483);
#1128=LINE('',#18890,#1484);
#1129=LINE('',#19033,#1485);
#1130=LINE('',#19056,#1486);
#1131=LINE('',#19076,#1487);
#1132=LINE('',#19078,#1488);
#1133=LINE('',#19080,#1489);
#1134=LINE('',#19081,#1490);
#1135=LINE('',#19083,#1491);
#1136=LINE('',#19234,#1492);
#1137=LINE('',#19236,#1493);
#1138=LINE('',#19393,#1494);
#1139=LINE('',#19404,#1495);
#1140=LINE('',#19406,#1496);
#1141=LINE('',#19410,#1497);
#1142=LINE('',#19412,#1498);
#1143=LINE('',#19413,#1499);
#1144=LINE('',#19416,#1500);
#1145=LINE('',#19417,#1501);
#1146=LINE('',#19420,#1502);
#1147=LINE('',#19421,#1503);
#1148=LINE('',#19424,#1504);
#1149=LINE('',#19425,#1505);
#1150=LINE('',#19428,#1506);
#1151=LINE('',#19429,#1507);
#1152=LINE('',#19431,#1508);
#1153=LINE('',#19435,#1509);
#1154=LINE('',#19436,#1510);
#1155=LINE('',#19437,#1511);
#1156=LINE('',#19440,#1512);
#1157=LINE('',#19441,#1513);
#1158=LINE('',#19444,#1514);
#1159=LINE('',#19445,#1515);
#1160=LINE('',#19448,#1516);
#1161=LINE('',#19449,#1517);
#1162=LINE('',#19452,#1518);
#1163=LINE('',#19453,#1519);
#1164=LINE('',#19455,#1520);
#1165=LINE('',#19460,#1521);
#1166=LINE('',#19467,#1522);
#1167=LINE('',#19478,#1523);
#1168=LINE('',#19480,#1524);
#1169=LINE('',#19484,#1525);
#1170=LINE('',#19486,#1526);
#1171=LINE('',#19487,#1527);
#1172=LINE('',#19490,#1528);
#1173=LINE('',#19491,#1529);
#1174=LINE('',#19494,#1530);
#1175=LINE('',#19495,#1531);
#1176=LINE('',#19498,#1532);
#1177=LINE('',#19499,#1533);
#1178=LINE('',#19502,#1534);
#1179=LINE('',#19503,#1535);
#1180=LINE('',#19505,#1536);
#1181=LINE('',#19509,#1537);
#1182=LINE('',#19510,#1538);
#1183=LINE('',#19511,#1539);
#1184=LINE('',#19514,#1540);
#1185=LINE('',#19515,#1541);
#1186=LINE('',#19518,#1542);
#1187=LINE('',#19519,#1543);
#1188=LINE('',#19522,#1544);
#1189=LINE('',#19523,#1545);
#1190=LINE('',#19526,#1546);
#1191=LINE('',#19527,#1547);
#1192=LINE('',#19529,#1548);
#1193=LINE('',#19534,#1549);
#1194=LINE('',#19541,#1550);
#1195=LINE('',#19553,#1551);
#1196=LINE('',#19560,#1552);
#1197=LINE('',#19572,#1553);
#1198=LINE('',#19589,#1554);
#1199=LINE('',#19596,#1555);
#1200=LINE('',#19602,#1556);
#1201=LINE('',#19613,#1557);
#1202=LINE('',#19620,#1558);
#1203=LINE('',#19627,#1559);
#1204=LINE('',#19635,#1560);
#1205=LINE('',#19638,#1561);
#1206=LINE('',#19653,#1562);
#1207=LINE('',#19656,#1563);
#1208=LINE('',#19661,#1564);
#1209=LINE('',#19663,#1565);
#1210=LINE('',#19665,#1566);
#1211=LINE('',#19667,#1567);
#1212=LINE('',#19668,#1568);
#1213=LINE('',#19672,#1569);
#1214=LINE('',#19677,#1570);
#1215=LINE('',#19680,#1571);
#1216=LINE('',#19686,#1572);
#1217=LINE('',#19689,#1573);
#1218=LINE('',#19691,#1574);
#1219=LINE('',#19693,#1575);
#1220=LINE('',#19694,#1576);
#1221=LINE('',#19702,#1577);
#1222=LINE('',#19708,#1578);
#1223=LINE('',#19712,#1579);
#1224=LINE('',#19716,#1580);
#1225=LINE('',#19719,#1581);
#1226=LINE('',#19720,#1582);
#1227=LINE('',#19729,#1583);
#1228=LINE('',#19735,#1584);
#1229=LINE('',#19742,#1585);
#1230=LINE('',#19745,#1586);
#1231=LINE('',#19760,#1587);
#1232=LINE('',#19763,#1588);
#1233=LINE('',#19767,#1589);
#1234=LINE('',#19769,#1590);
#1235=LINE('',#19771,#1591);
#1236=LINE('',#19772,#1592);
#1237=LINE('',#19775,#1593);
#1238=LINE('',#19779,#1594);
#1239=LINE('',#19783,#1595);
#1240=LINE('',#19789,#1596);
#1241=LINE('',#19792,#1597);
#1242=LINE('',#19794,#1598);
#1243=LINE('',#19795,#1599);
#1244=LINE('',#19803,#1600);
#1245=LINE('',#19809,#1601);
#1246=LINE('',#19812,#1602);
#1247=LINE('',#19816,#1603);
#1248=LINE('',#19820,#1604);
#1249=LINE('',#19821,#1605);
#1250=LINE('',#19830,#1606);
#1251=LINE('',#19840,#1607);
#1252=LINE('',#19847,#1608);
#1253=VECTOR('',#5435,5.);
#1254=VECTOR('',#5442,10.);
#1255=VECTOR('',#5445,10.);
#1256=VECTOR('',#5448,10.);
#1257=VECTOR('',#5449,10.);
#1258=VECTOR('',#5450,10.);
#1259=VECTOR('',#5455,10.);
#1260=VECTOR('',#5458,10.);
#1261=VECTOR('',#5461,10.);
#1262=VECTOR('',#5462,10.);
#1263=VECTOR('',#5463,10.);
#1264=VECTOR('',#5468,10.);
#1265=VECTOR('',#5471,10.);
#1266=VECTOR('',#5474,10.);
#1267=VECTOR('',#5475,10.);
#1268=VECTOR('',#5476,10.);
#1269=VECTOR('',#5481,10.);
#1270=VECTOR('',#5484,10.);
#1271=VECTOR('',#5487,10.);
#1272=VECTOR('',#5488,10.);
#1273=VECTOR('',#5489,10.);
#1274=VECTOR('',#5494,10.);
#1275=VECTOR('',#5497,10.);
#1276=VECTOR('',#5500,10.);
#1277=VECTOR('',#5501,10.);
#1278=VECTOR('',#5502,10.);
#1279=VECTOR('',#5507,10.);
#1280=VECTOR('',#5510,10.);
#1281=VECTOR('',#5513,10.);
#1282=VECTOR('',#5514,10.);
#1283=VECTOR('',#5515,10.);
#1284=VECTOR('',#5520,10.);
#1285=VECTOR('',#5523,10.);
#1286=VECTOR('',#5526,10.);
#1287=VECTOR('',#5527,10.);
#1288=VECTOR('',#5528,10.);
#1289=VECTOR('',#5533,10.);
#1290=VECTOR('',#5536,10.);
#1291=VECTOR('',#5539,10.);
#1292=VECTOR('',#5540,10.);
#1293=VECTOR('',#5541,10.);
#1294=VECTOR('',#5546,10.);
#1295=VECTOR('',#5549,10.);
#1296=VECTOR('',#5552,10.);
#1297=VECTOR('',#5553,10.);
#1298=VECTOR('',#5554,10.);
#1299=VECTOR('',#5559,10.);
#1300=VECTOR('',#5562,10.);
#1301=VECTOR('',#5565,10.);
#1302=VECTOR('',#5566,10.);
#1303=VECTOR('',#5567,10.);
#1304=VECTOR('',#5572,10.);
#1305=VECTOR('',#5575,10.);
#1306=VECTOR('',#5578,10.);
#1307=VECTOR('',#5579,10.);
#1308=VECTOR('',#5580,10.);
#1309=VECTOR('',#5585,10.);
#1310=VECTOR('',#5588,10.);
#1311=VECTOR('',#5591,10.);
#1312=VECTOR('',#5592,10.);
#1313=VECTOR('',#5593,10.);
#1314=VECTOR('',#5598,10.);
#1315=VECTOR('',#5601,10.);
#1316=VECTOR('',#5604,10.);
#1317=VECTOR('',#5605,10.);
#1318=VECTOR('',#5606,10.);
#1319=VECTOR('',#5611,10.);
#1320=VECTOR('',#5614,10.);
#1321=VECTOR('',#5617,10.);
#1322=VECTOR('',#5618,10.);
#1323=VECTOR('',#5619,10.);
#1324=VECTOR('',#5624,10.);
#1325=VECTOR('',#5627,10.);
#1326=VECTOR('',#5630,10.);
#1327=VECTOR('',#5631,10.);
#1328=VECTOR('',#5632,10.);
#1329=VECTOR('',#5637,10.);
#1330=VECTOR('',#5640,10.);
#1331=VECTOR('',#5643,10.);
#1332=VECTOR('',#5644,10.);
#1333=VECTOR('',#5645,10.);
#1334=VECTOR('',#5650,10.);
#1335=VECTOR('',#5653,10.);
#1336=VECTOR('',#5656,10.);
#1337=VECTOR('',#5657,10.);
#1338=VECTOR('',#5658,10.);
#1339=VECTOR('',#5663,10.);
#1340=VECTOR('',#5666,10.);
#1341=VECTOR('',#5669,10.);
#1342=VECTOR('',#5670,10.);
#1343=VECTOR('',#5671,10.);
#1344=VECTOR('',#5676,10.);
#1345=VECTOR('',#5679,10.);
#1346=VECTOR('',#5682,10.);
#1347=VECTOR('',#5683,10.);
#1348=VECTOR('',#5684,10.);
#1349=VECTOR('',#5689,10.);
#1350=VECTOR('',#5692,10.);
#1351=VECTOR('',#5695,10.);
#1352=VECTOR('',#5696,10.);
#1353=VECTOR('',#5697,10.);
#1354=VECTOR('',#5702,10.);
#1355=VECTOR('',#5705,10.);
#1356=VECTOR('',#5708,10.);
#1357=VECTOR('',#5709,10.);
#1358=VECTOR('',#5710,10.);
#1359=VECTOR('',#5715,10.);
#1360=VECTOR('',#5718,10.);
#1361=VECTOR('',#5721,10.);
#1362=VECTOR('',#5722,10.);
#1363=VECTOR('',#5723,10.);
#1364=VECTOR('',#5728,10.);
#1365=VECTOR('',#5731,10.);
#1366=VECTOR('',#5734,10.);
#1367=VECTOR('',#5735,10.);
#1368=VECTOR('',#5736,10.);
#1369=VECTOR('',#5741,10.);
#1370=VECTOR('',#5744,10.);
#1371=VECTOR('',#5747,10.);
#1372=VECTOR('',#5748,10.);
#1373=VECTOR('',#5749,10.);
#1374=VECTOR('',#5754,10.);
#1375=VECTOR('',#5757,10.);
#1376=VECTOR('',#5760,10.);
#1377=VECTOR('',#5761,10.);
#1378=VECTOR('',#5762,10.);
#1379=VECTOR('',#5767,10.);
#1380=VECTOR('',#5770,10.);
#1381=VECTOR('',#5773,10.);
#1382=VECTOR('',#5774,10.);
#1383=VECTOR('',#5775,10.);
#1384=VECTOR('',#5780,10.);
#1385=VECTOR('',#5783,10.);
#1386=VECTOR('',#5786,10.);
#1387=VECTOR('',#5787,10.);
#1388=VECTOR('',#5788,10.);
#1389=VECTOR('',#5793,10.);
#1390=VECTOR('',#5796,10.);
#1391=VECTOR('',#5799,10.);
#1392=VECTOR('',#5800,10.);
#1393=VECTOR('',#5801,10.);
#1394=VECTOR('',#5806,10.);
#1395=VECTOR('',#5809,10.);
#1396=VECTOR('',#5812,10.);
#1397=VECTOR('',#5813,10.);
#1398=VECTOR('',#5814,10.);
#1399=VECTOR('',#5819,10.);
#1400=VECTOR('',#5822,10.);
#1401=VECTOR('',#5825,10.);
#1402=VECTOR('',#5826,10.);
#1403=VECTOR('',#5827,10.);
#1404=VECTOR('',#5832,10.);
#1405=VECTOR('',#5835,10.);
#1406=VECTOR('',#5838,10.);
#1407=VECTOR('',#5839,10.);
#1408=VECTOR('',#5840,10.);
#1409=VECTOR('',#5845,10.);
#1410=VECTOR('',#5848,10.);
#1411=VECTOR('',#5851,10.);
#1412=VECTOR('',#5852,10.);
#1413=VECTOR('',#5853,10.);
#1414=VECTOR('',#5858,10.);
#1415=VECTOR('',#5861,10.);
#1416=VECTOR('',#5864,10.);
#1417=VECTOR('',#5865,10.);
#1418=VECTOR('',#5866,10.);
#1419=VECTOR('',#5871,10.);
#1420=VECTOR('',#5874,10.);
#1421=VECTOR('',#5877,10.);
#1422=VECTOR('',#5878,10.);
#1423=VECTOR('',#5879,10.);
#1424=VECTOR('',#5884,10.);
#1425=VECTOR('',#5887,10.);
#1426=VECTOR('',#5890,10.);
#1427=VECTOR('',#5891,10.);
#1428=VECTOR('',#5892,10.);
#1429=VECTOR('',#5897,10.);
#1430=VECTOR('',#5900,10.);
#1431=VECTOR('',#5903,10.);
#1432=VECTOR('',#5904,10.);
#1433=VECTOR('',#5905,10.);
#1434=VECTOR('',#5910,10.);
#1435=VECTOR('',#5913,10.);
#1436=VECTOR('',#5916,10.);
#1437=VECTOR('',#5917,10.);
#1438=VECTOR('',#5918,10.);
#1439=VECTOR('',#5923,10.);
#1440=VECTOR('',#5926,10.);
#1441=VECTOR('',#5929,10.);
#1442=VECTOR('',#5930,10.);
#1443=VECTOR('',#5931,10.);
#1444=VECTOR('',#5932,10.);
#1445=VECTOR('',#5939,10.);
#1446=VECTOR('',#5940,10.);
#1447=VECTOR('',#5947,10.);
#1448=VECTOR('',#5948,10.);
#1449=VECTOR('',#5955,10.);
#1450=VECTOR('',#5956,10.);
#1451=VECTOR('',#5963,10.);
#1452=VECTOR('',#5964,10.);
#1453=VECTOR('',#5971,10.);
#1454=VECTOR('',#5972,10.);
#1455=VECTOR('',#5979,10.);
#1456=VECTOR('',#5980,10.);
#1457=VECTOR('',#5987,10.);
#1458=VECTOR('',#5988,10.);
#1459=VECTOR('',#5995,10.);
#1460=VECTOR('',#5996,10.);
#1461=VECTOR('',#6003,10.);
#1462=VECTOR('',#6004,10.);
#1463=VECTOR('',#6011,10.);
#1464=VECTOR('',#6012,10.);
#1465=VECTOR('',#6019,10.);
#1466=VECTOR('',#6020,10.);
#1467=VECTOR('',#6027,10.);
#1468=VECTOR('',#6028,10.);
#1469=VECTOR('',#6035,10.);
#1470=VECTOR('',#6036,10.);
#1471=VECTOR('',#6043,10.);
#1472=VECTOR('',#6044,10.);
#1473=VECTOR('',#6051,10.);
#1474=VECTOR('',#6052,10.);
#1475=VECTOR('',#6059,10.);
#1476=VECTOR('',#6060,10.);
#1477=VECTOR('',#6067,10.);
#1478=VECTOR('',#6068,10.);
#1479=VECTOR('',#6075,10.);
#1480=VECTOR('',#6076,10.);
#1481=VECTOR('',#6083,10.);
#1482=VECTOR('',#6124,10.);
#1483=VECTOR('',#6127,10.);
#1484=VECTOR('',#6140,10.);
#1485=VECTOR('',#6143,10.);
#1486=VECTOR('',#6186,10.);
#1487=VECTOR('',#6225,10.);
#1488=VECTOR('',#6228,10.);
#1489=VECTOR('',#6231,10.);
#1490=VECTOR('',#6232,10.);
#1491=VECTOR('',#6235,10.);
#1492=VECTOR('',#6236,10.);
#1493=VECTOR('',#6239,10.);
#1494=VECTOR('',#6248,7.28);
#1495=VECTOR('',#6263,11.24);
#1496=VECTOR('',#6266,7.911);
#1497=VECTOR('',#6269,10.);
#1498=VECTOR('',#6270,10.);
#1499=VECTOR('',#6271,10.);
#1500=VECTOR('',#6274,10.);
#1501=VECTOR('',#6275,10.);
#1502=VECTOR('',#6278,10.);
#1503=VECTOR('',#6279,10.);
#1504=VECTOR('',#6282,9.99999999999999);
#1505=VECTOR('',#6283,10.);
#1506=VECTOR('',#6286,10.);
#1507=VECTOR('',#6287,10.);
#1508=VECTOR('',#6290,10.);
#1509=VECTOR('',#6293,10.);
#1510=VECTOR('',#6294,10.);
#1511=VECTOR('',#6295,10.);
#1512=VECTOR('',#6298,10.);
#1513=VECTOR('',#6299,10.);
#1514=VECTOR('',#6302,10.);
#1515=VECTOR('',#6303,10.);
#1516=VECTOR('',#6306,9.99999999999999);
#1517=VECTOR('',#6307,10.);
#1518=VECTOR('',#6310,10.);
#1519=VECTOR('',#6311,10.);
#1520=VECTOR('',#6314,10.);
#1521=VECTOR('',#6321,14.48);
#1522=VECTOR('',#6330,7.28);
#1523=VECTOR('',#6345,11.24);
#1524=VECTOR('',#6348,7.911);
#1525=VECTOR('',#6351,10.);
#1526=VECTOR('',#6352,10.);
#1527=VECTOR('',#6353,10.);
#1528=VECTOR('',#6356,10.);
#1529=VECTOR('',#6357,10.);
#1530=VECTOR('',#6360,10.);
#1531=VECTOR('',#6361,10.);
#1532=VECTOR('',#6364,9.99999999999999);
#1533=VECTOR('',#6365,10.);
#1534=VECTOR('',#6368,10.);
#1535=VECTOR('',#6369,10.);
#1536=VECTOR('',#6372,10.);
#1537=VECTOR('',#6375,10.);
#1538=VECTOR('',#6376,10.);
#1539=VECTOR('',#6377,10.);
#1540=VECTOR('',#6380,10.);
#1541=VECTOR('',#6381,10.);
#1542=VECTOR('',#6384,10.);
#1543=VECTOR('',#6385,10.);
#1544=VECTOR('',#6388,9.99999999999999);
#1545=VECTOR('',#6389,10.);
#1546=VECTOR('',#6392,10.);
#1547=VECTOR('',#6393,10.);
#1548=VECTOR('',#6396,10.);
#1549=VECTOR('',#6403,14.48);
#1550=VECTOR('',#6412,5.);
#1551=VECTOR('',#6429,11.);
#1552=VECTOR('',#6438,27.4027293621977);
#1553=VECTOR('',#6455,19.7498324643894);
#1554=VECTOR('',#6478,26.6934256722844);
#1555=VECTOR('',#6487,33.);
#1556=VECTOR('',#6496,11.);
#1557=VECTOR('',#6511,27.4027293621977);
#1558=VECTOR('',#6520,29.0578798664922);
#1559=VECTOR('',#6529,31.1192710879259);
#1560=VECTOR('',#6538,10.);
#1561=VECTOR('',#6541,10.);
#1562=VECTOR('',#6560,10.);
#1563=VECTOR('',#6563,10.);
#1564=VECTOR('',#6570,10.);
#1565=VECTOR('',#6571,10.);
#1566=VECTOR('',#6572,10.);
#1567=VECTOR('',#6573,10.);
#1568=VECTOR('',#6574,10.);
#1569=VECTOR('',#6579,10.);
#1570=VECTOR('',#6584,10.);
#1571=VECTOR('',#6587,10.);
#1572=VECTOR('',#6594,10.);
#1573=VECTOR('',#6597,10.);
#1574=VECTOR('',#6598,10.);
#1575=VECTOR('',#6599,10.);
#1576=VECTOR('',#6600,10.);
#1577=VECTOR('',#6611,10.);
#1578=VECTOR('',#6620,9.8273485245745);
#1579=VECTOR('',#6625,8.8273485245745);
#1580=VECTOR('',#6630,10.);
#1581=VECTOR('',#6633,10.);
#1582=VECTOR('',#6634,10.);
#1583=VECTOR('',#6647,10.);
#1584=VECTOR('',#6654,10.);
#1585=VECTOR('',#6661,10.);
#1586=VECTOR('',#6664,10.);
#1587=VECTOR('',#6683,10.);
#1588=VECTOR('',#6686,10.);
#1589=VECTOR('',#6693,10.);
#1590=VECTOR('',#6694,10.);
#1591=VECTOR('',#6695,10.);
#1592=VECTOR('',#6696,10.);
#1593=VECTOR('',#6699,10.);
#1594=VECTOR('',#6704,10.);
#1595=VECTOR('',#6707,10.);
#1596=VECTOR('',#6714,10.);
#1597=VECTOR('',#6719,10.);
#1598=VECTOR('',#6720,10.);
#1599=VECTOR('',#6721,10.);
#1600=VECTOR('',#6732,10.);
#1601=VECTOR('',#6741,9.8273485245745);
#1602=VECTOR('',#6744,8.8273485245745);
#1603=VECTOR('',#6749,10.);
#1604=VECTOR('',#6754,10.);
#1605=VECTOR('',#6755,10.);
#1606=VECTOR('',#6768,27.4027293621977);
#1607=VECTOR('',#6783,31.1192710879259);
#1608=VECTOR('',#6792,29.0578798664922);
#1609=CIRCLE('',#4913,5.);
#1610=CIRCLE('',#4914,5.);
#1611=CIRCLE('',#4916,1.);
#1612=CIRCLE('',#4917,1.);
#1613=CIRCLE('',#4920,1.);
#1614=CIRCLE('',#4921,1.);
#1615=CIRCLE('',#4924,1.);
#1616=CIRCLE('',#4925,1.);
#1617=CIRCLE('',#4928,1.);
#1618=CIRCLE('',#4929,1.);
#1619=CIRCLE('',#4932,1.);
#1620=CIRCLE('',#4933,1.);
#1621=CIRCLE('',#4936,1.);
#1622=CIRCLE('',#4937,1.);
#1623=CIRCLE('',#4940,1.);
#1624=CIRCLE('',#4941,1.);
#1625=CIRCLE('',#4944,1.);
#1626=CIRCLE('',#4945,1.);
#1627=CIRCLE('',#4948,1.);
#1628=CIRCLE('',#4949,1.);
#1629=CIRCLE('',#4952,1.);
#1630=CIRCLE('',#4953,1.);
#1631=CIRCLE('',#4956,1.);
#1632=CIRCLE('',#4957,1.);
#1633=CIRCLE('',#4960,1.);
#1634=CIRCLE('',#4961,1.);
#1635=CIRCLE('',#4964,1.);
#1636=CIRCLE('',#4965,1.);
#1637=CIRCLE('',#4968,1.);
#1638=CIRCLE('',#4969,1.);
#1639=CIRCLE('',#4972,1.);
#1640=CIRCLE('',#4973,1.);
#1641=CIRCLE('',#4976,1.);
#1642=CIRCLE('',#4977,1.);
#1643=CIRCLE('',#4980,1.);
#1644=CIRCLE('',#4981,1.);
#1645=CIRCLE('',#4984,1.);
#1646=CIRCLE('',#4985,1.);
#1647=CIRCLE('',#4988,1.);
#1648=CIRCLE('',#4989,1.);
#1649=CIRCLE('',#4992,1.);
#1650=CIRCLE('',#4993,1.);
#1651=CIRCLE('',#4996,1.);
#1652=CIRCLE('',#4997,1.);
#1653=CIRCLE('',#5000,1.);
#1654=CIRCLE('',#5001,1.);
#1655=CIRCLE('',#5004,1.);
#1656=CIRCLE('',#5005,1.);
#1657=CIRCLE('',#5008,1.);
#1658=CIRCLE('',#5009,1.);
#1659=CIRCLE('',#5012,1.);
#1660=CIRCLE('',#5013,1.);
#1661=CIRCLE('',#5016,1.);
#1662=CIRCLE('',#5017,1.);
#1663=CIRCLE('',#5020,1.);
#1664=CIRCLE('',#5021,1.);
#1665=CIRCLE('',#5024,1.);
#1666=CIRCLE('',#5025,1.);
#1667=CIRCLE('',#5028,1.);
#1668=CIRCLE('',#5029,1.);
#1669=CIRCLE('',#5032,1.);
#1670=CIRCLE('',#5033,1.);
#1671=CIRCLE('',#5036,1.);
#1672=CIRCLE('',#5037,1.);
#1673=CIRCLE('',#5040,1.);
#1674=CIRCLE('',#5041,1.);
#1675=CIRCLE('',#5044,1.);
#1676=CIRCLE('',#5045,1.);
#1677=CIRCLE('',#5048,1.);
#1678=CIRCLE('',#5049,1.);
#1679=CIRCLE('',#5052,1.);
#1680=CIRCLE('',#5053,1.);
#1681=CIRCLE('',#5056,1.);
#1682=CIRCLE('',#5057,1.);
#1683=CIRCLE('',#5060,1.);
#1684=CIRCLE('',#5061,1.);
#1685=CIRCLE('',#5064,1.);
#1686=CIRCLE('',#5065,1.);
#1687=CIRCLE('',#5068,21.9999999999943);
#1688=CIRCLE('',#5069,21.9999999999943);
#1689=CIRCLE('',#5071,21.9999999999943);
#1690=CIRCLE('',#5072,21.9999999999943);
#1691=CIRCLE('',#5074,21.9999999999943);
#1692=CIRCLE('',#5075,21.9999999999943);
#1693=CIRCLE('',#5077,21.9999999999943);
#1694=CIRCLE('',#5078,21.9999999999943);
#1695=CIRCLE('',#5080,21.9999999999943);
#1696=CIRCLE('',#5081,21.9999999999943);
#1697=CIRCLE('',#5083,21.9999999999943);
#1698=CIRCLE('',#5084,21.9999999999943);
#1699=CIRCLE('',#5086,21.9999999999943);
#1700=CIRCLE('',#5087,21.9999999999943);
#1701=CIRCLE('',#5089,21.9999999999943);
#1702=CIRCLE('',#5090,21.9999999999943);
#1703=CIRCLE('',#5092,21.9999999999943);
#1704=CIRCLE('',#5093,21.9999999999943);
#1705=CIRCLE('',#5095,21.9999999999943);
#1706=CIRCLE('',#5096,21.9999999999943);
#1707=CIRCLE('',#5098,21.9999999999943);
#1708=CIRCLE('',#5099,21.9999999999943);
#1709=CIRCLE('',#5101,21.9999999999943);
#1710=CIRCLE('',#5102,21.9999999999943);
#1711=CIRCLE('',#5104,21.9999999999943);
#1712=CIRCLE('',#5105,21.9999999999943);
#1713=CIRCLE('',#5107,21.9999999999943);
#1714=CIRCLE('',#5108,21.9999999999943);
#1715=CIRCLE('',#5110,21.9999999999943);
#1716=CIRCLE('',#5111,21.9999999999943);
#1717=CIRCLE('',#5113,21.9999999999943);
#1718=CIRCLE('',#5114,21.9999999999943);
#1719=CIRCLE('',#5116,21.9999999999943);
#1720=CIRCLE('',#5117,21.9999999999943);
#1721=CIRCLE('',#5119,21.9999999999943);
#1722=CIRCLE('',#5120,21.9999999999943);
#1723=CIRCLE('',#5122,21.9999999999943);
#1724=CIRCLE('',#5123,21.9999999999943);
#1725=CIRCLE('',#5125,17.686);
#1726=CIRCLE('',#5126,17.686);
#1727=CIRCLE('',#5127,17.686);
#1728=CIRCLE('',#5128,17.686);
#1729=CIRCLE('',#5129,17.686);
#1730=CIRCLE('',#5130,17.686);
#1731=CIRCLE('',#5131,17.686);
#1732=CIRCLE('',#5132,17.686);
#1733=CIRCLE('',#5133,17.686);
#1734=CIRCLE('',#5134,17.686);
#1735=CIRCLE('',#5135,17.686);
#1736=CIRCLE('',#5136,17.686);
#1737=CIRCLE('',#5137,17.686);
#1738=CIRCLE('',#5138,17.686);
#1739=CIRCLE('',#5139,17.686);
#1740=CIRCLE('',#5140,17.686);
#1741=CIRCLE('',#5141,17.686);
#1742=CIRCLE('',#5142,17.686);
#1743=CIRCLE('',#5143,1.);
#1744=CIRCLE('',#5144,21.9999999999943);
#1745=CIRCLE('',#5145,1.);
#1746=CIRCLE('',#5146,17.686);
#1747=CIRCLE('',#5147,17.686);
#1748=CIRCLE('',#5149,17.686);
#1749=CIRCLE('',#5150,1.);
#1750=CIRCLE('',#5151,21.9999999999943);
#1751=CIRCLE('',#5152,1.);
#1752=CIRCLE('',#5153,17.686);
#1753=CIRCLE('',#5154,17.686);
#1754=CIRCLE('',#5155,17.686);
#1755=CIRCLE('',#5156,17.686);
#1756=CIRCLE('',#5157,17.686);
#1757=CIRCLE('',#5158,17.686);
#1758=CIRCLE('',#5159,17.686);
#1759=CIRCLE('',#5160,17.686);
#1760=CIRCLE('',#5161,17.686);
#1761=CIRCLE('',#5162,17.686);
#1762=CIRCLE('',#5163,17.686);
#1763=CIRCLE('',#5164,17.686);
#1764=CIRCLE('',#5165,17.686);
#1765=CIRCLE('',#5166,17.686);
#1766=CIRCLE('',#5167,17.686);
#1767=CIRCLE('',#5168,17.686);
#1768=CIRCLE('',#5169,17.686);
#1769=CIRCLE('',#5170,17.686);
#1770=CIRCLE('',#5171,17.686);
#1771=CIRCLE('',#5199,7.911);
#1772=CIRCLE('',#5200,6.4);
#1773=CIRCLE('',#5202,7.911);
#1774=CIRCLE('',#5203,1.);
#1775=CIRCLE('',#5204,8.20389321881349);
#1776=CIRCLE('',#5206,14.48);
#1777=CIRCLE('',#5221,14.48);
#1778=CIRCLE('',#5226,7.911);
#1779=CIRCLE('',#5227,6.4);
#1780=CIRCLE('',#5229,7.911);
#1781=CIRCLE('',#5230,1.);
#1782=CIRCLE('',#5231,8.20389321881349);
#1783=CIRCLE('',#5233,14.48);
#1784=CIRCLE('',#5248,14.48);
#1785=CIRCLE('',#5253,5.);
#1786=CIRCLE('',#5254,5.);
#1787=CIRCLE('',#5256,11.);
#1788=CIRCLE('',#5258,11.);
#1789=CIRCLE('',#5259,1.);
#1790=CIRCLE('',#5260,12.8892103004758);
#1791=CIRCLE('',#5263,27.4027293621977);
#1792=CIRCLE('',#5265,27.4027293621977);
#1793=CIRCLE('',#5270,18.2498324643894);
#1794=CIRCLE('',#5271,1.5);
#1795=CIRCLE('',#5272,19.7498324643894);
#1796=CIRCLE('',#5274,19.7498324643894);
#1797=CIRCLE('',#5276,11.);
#1798=CIRCLE('',#5278,26.6934256722844);
#1799=CIRCLE('',#5279,1.5);
#1800=CIRCLE('',#5280,28.1934256722844);
#1801=CIRCLE('',#5282,31.5);
#1802=CIRCLE('',#5284,26.6934256722844);
#1803=CIRCLE('',#5286,1.5);
#1804=CIRCLE('',#5287,33.);
#1805=CIRCLE('',#5289,33.);
#1806=CIRCLE('',#5292,11.);
#1807=CIRCLE('',#5294,12.8892103004758);
#1808=CIRCLE('',#5295,1.);
#1809=CIRCLE('',#5297,27.4027293621977);
#1810=CIRCLE('',#5299,27.4027293621977);
#1811=CIRCLE('',#5301,29.0578798664922);
#1812=CIRCLE('',#5303,29.0578798664922);
#1813=CIRCLE('',#5305,31.1192710879259);
#1814=CIRCLE('',#5307,31.1192710879259);
#1815=CIRCLE('',#5311,0.999999999999996);
#1816=CIRCLE('',#5312,1.);
#1817=CIRCLE('',#5314,0.999999999999999);
#1818=CIRCLE('',#5315,38.889325151227);
#1819=CIRCLE('',#5316,1.);
#1820=CIRCLE('',#5317,39.889325151227);
#1821=CIRCLE('',#5319,1.);
#1822=CIRCLE('',#5321,1.);
#1823=CIRCLE('',#5322,1.);
#1824=CIRCLE('',#5324,1.);
#1825=CIRCLE('',#5327,1.);
#1826=CIRCLE('',#5329,4.);
#1827=CIRCLE('',#5330,4.);
#1828=CIRCLE('',#5331,10.8273485245745);
#1829=CIRCLE('',#5333,1.);
#1830=CIRCLE('',#5336,1.);
#1831=CIRCLE('',#5337,5.);
#1832=CIRCLE('',#5339,1.);
#1833=CIRCLE('',#5341,5.);
#1834=CIRCLE('',#5343,8.8273485245745);
#1835=CIRCLE('',#5345,8.8273485245745);
#1836=CIRCLE('',#5347,5.);
#1837=CIRCLE('',#5350,5.);
#1838=CIRCLE('',#5352,38.889325151227);
#1839=CIRCLE('',#5354,33.);
#1840=CIRCLE('',#5355,33.);
#1841=CIRCLE('',#5357,33.);
#1842=CIRCLE('',#5358,33.);
#1843=CIRCLE('',#5360,0.999999999999996);
#1844=CIRCLE('',#5361,1.);
#1845=CIRCLE('',#5363,0.999999999999999);
#1846=CIRCLE('',#5364,39.889325151227);
#1847=CIRCLE('',#5365,1.);
#1848=CIRCLE('',#5366,38.889325151227);
#1849=CIRCLE('',#5368,1.);
#1850=CIRCLE('',#5370,1.);
#1851=CIRCLE('',#5371,1.);
#1852=CIRCLE('',#5373,1.);
#1853=CIRCLE('',#5376,1.);
#1854=CIRCLE('',#5378,4.);
#1855=CIRCLE('',#5379,4.);
#1856=CIRCLE('',#5380,10.8273485245745);
#1857=CIRCLE('',#5382,1.);
#1858=CIRCLE('',#5385,1.);
#1859=CIRCLE('',#5386,5.);
#1860=CIRCLE('',#5388,1.);
#1861=CIRCLE('',#5390,5.);
#1862=CIRCLE('',#5392,8.8273485245745);
#1863=CIRCLE('',#5394,8.8273485245745);
#1864=CIRCLE('',#5396,5.);
#1865=CIRCLE('',#5399,5.);
#1866=CIRCLE('',#5401,38.889325151227);
#1867=CIRCLE('',#5403,27.4027293621977);
#1868=CIRCLE('',#5404,27.4027293621977);
#1869=CIRCLE('',#5408,31.1192710879259);
#1870=CIRCLE('',#5410,31.1192710879259);
#1871=CIRCLE('',#5412,29.0578798664922);
#1872=CIRCLE('',#5414,29.0578798664922);
#1873=CIRCLE('',#5418,1.);
#1874=CIRCLE('',#5419,11.);
#1875=VERTEX_POINT('',#6820);
#1876=VERTEX_POINT('',#6822);
#1877=VERTEX_POINT('',#6826);
#1878=VERTEX_POINT('',#6827);
#1879=VERTEX_POINT('',#6829);
#1880=VERTEX_POINT('',#6831);
#1881=VERTEX_POINT('',#6835);
#1882=VERTEX_POINT('',#6837);
#1883=VERTEX_POINT('',#6841);
#1884=VERTEX_POINT('',#6842);
#1885=VERTEX_POINT('',#6844);
#1886=VERTEX_POINT('',#6846);
#1887=VERTEX_POINT('',#6850);
#1888=VERTEX_POINT('',#6852);
#1889=VERTEX_POINT('',#6856);
#1890=VERTEX_POINT('',#6857);
#1891=VERTEX_POINT('',#6859);
#1892=VERTEX_POINT('',#6861);
#1893=VERTEX_POINT('',#6865);
#1894=VERTEX_POINT('',#6867);
#1895=VERTEX_POINT('',#6871);
#1896=VERTEX_POINT('',#6872);
#1897=VERTEX_POINT('',#6874);
#1898=VERTEX_POINT('',#6876);
#1899=VERTEX_POINT('',#6880);
#1900=VERTEX_POINT('',#6882);
#1901=VERTEX_POINT('',#6886);
#1902=VERTEX_POINT('',#6887);
#1903=VERTEX_POINT('',#6889);
#1904=VERTEX_POINT('',#6891);
#1905=VERTEX_POINT('',#6895);
#1906=VERTEX_POINT('',#6897);
#1907=VERTEX_POINT('',#6901);
#1908=VERTEX_POINT('',#6902);
#1909=VERTEX_POINT('',#6904);
#1910=VERTEX_POINT('',#6906);
#1911=VERTEX_POINT('',#6910);
#1912=VERTEX_POINT('',#6912);
#1913=VERTEX_POINT('',#6916);
#1914=VERTEX_POINT('',#6917);
#1915=VERTEX_POINT('',#6919);
#1916=VERTEX_POINT('',#6921);
#1917=VERTEX_POINT('',#6925);
#1918=VERTEX_POINT('',#6927);
#1919=VERTEX_POINT('',#6931);
#1920=VERTEX_POINT('',#6932);
#1921=VERTEX_POINT('',#6934);
#1922=VERTEX_POINT('',#6936);
#1923=VERTEX_POINT('',#6940);
#1924=VERTEX_POINT('',#6942);
#1925=VERTEX_POINT('',#6946);
#1926=VERTEX_POINT('',#6947);
#1927=VERTEX_POINT('',#6949);
#1928=VERTEX_POINT('',#6951);
#1929=VERTEX_POINT('',#6955);
#1930=VERTEX_POINT('',#6957);
#1931=VERTEX_POINT('',#6961);
#1932=VERTEX_POINT('',#6962);
#1933=VERTEX_POINT('',#6964);
#1934=VERTEX_POINT('',#6966);
#1935=VERTEX_POINT('',#6970);
#1936=VERTEX_POINT('',#6972);
#1937=VERTEX_POINT('',#6976);
#1938=VERTEX_POINT('',#6977);
#1939=VERTEX_POINT('',#6979);
#1940=VERTEX_POINT('',#6981);
#1941=VERTEX_POINT('',#6985);
#1942=VERTEX_POINT('',#6987);
#1943=VERTEX_POINT('',#6991);
#1944=VERTEX_POINT('',#6992);
#1945=VERTEX_POINT('',#6994);
#1946=VERTEX_POINT('',#6996);
#1947=VERTEX_POINT('',#7000);
#1948=VERTEX_POINT('',#7002);
#1949=VERTEX_POINT('',#7006);
#1950=VERTEX_POINT('',#7007);
#1951=VERTEX_POINT('',#7009);
#1952=VERTEX_POINT('',#7011);
#1953=VERTEX_POINT('',#7015);
#1954=VERTEX_POINT('',#7017);
#1955=VERTEX_POINT('',#7021);
#1956=VERTEX_POINT('',#7022);
#1957=VERTEX_POINT('',#7024);
#1958=VERTEX_POINT('',#7026);
#1959=VERTEX_POINT('',#7030);
#1960=VERTEX_POINT('',#7032);
#1961=VERTEX_POINT('',#7036);
#1962=VERTEX_POINT('',#7037);
#1963=VERTEX_POINT('',#7039);
#1964=VERTEX_POINT('',#7041);
#1965=VERTEX_POINT('',#7045);
#1966=VERTEX_POINT('',#7047);
#1967=VERTEX_POINT('',#7051);
#1968=VERTEX_POINT('',#7052);
#1969=VERTEX_POINT('',#7054);
#1970=VERTEX_POINT('',#7056);
#1971=VERTEX_POINT('',#7060);
#1972=VERTEX_POINT('',#7062);
#1973=VERTEX_POINT('',#7066);
#1974=VERTEX_POINT('',#7067);
#1975=VERTEX_POINT('',#7069);
#1976=VERTEX_POINT('',#7071);
#1977=VERTEX_POINT('',#7075);
#1978=VERTEX_POINT('',#7077);
#1979=VERTEX_POINT('',#7081);
#1980=VERTEX_POINT('',#7082);
#1981=VERTEX_POINT('',#7084);
#1982=VERTEX_POINT('',#7086);
#1983=VERTEX_POINT('',#7090);
#1984=VERTEX_POINT('',#7092);
#1985=VERTEX_POINT('',#7096);
#1986=VERTEX_POINT('',#7097);
#1987=VERTEX_POINT('',#7099);
#1988=VERTEX_POINT('',#7101);
#1989=VERTEX_POINT('',#7105);
#1990=VERTEX_POINT('',#7107);
#1991=VERTEX_POINT('',#7111);
#1992=VERTEX_POINT('',#7112);
#1993=VERTEX_POINT('',#7114);
#1994=VERTEX_POINT('',#7116);
#1995=VERTEX_POINT('',#7120);
#1996=VERTEX_POINT('',#7122);
#1997=VERTEX_POINT('',#7126);
#1998=VERTEX_POINT('',#7127);
#1999=VERTEX_POINT('',#7129);
#2000=VERTEX_POINT('',#7131);
#2001=VERTEX_POINT('',#7135);
#2002=VERTEX_POINT('',#7137);
#2003=VERTEX_POINT('',#7141);
#2004=VERTEX_POINT('',#7142);
#2005=VERTEX_POINT('',#7144);
#2006=VERTEX_POINT('',#7146);
#2007=VERTEX_POINT('',#7150);
#2008=VERTEX_POINT('',#7152);
#2009=VERTEX_POINT('',#7156);
#2010=VERTEX_POINT('',#7157);
#2011=VERTEX_POINT('',#7159);
#2012=VERTEX_POINT('',#7161);
#2013=VERTEX_POINT('',#7165);
#2014=VERTEX_POINT('',#7167);
#2015=VERTEX_POINT('',#7171);
#2016=VERTEX_POINT('',#7172);
#2017=VERTEX_POINT('',#7174);
#2018=VERTEX_POINT('',#7176);
#2019=VERTEX_POINT('',#7180);
#2020=VERTEX_POINT('',#7182);
#2021=VERTEX_POINT('',#7186);
#2022=VERTEX_POINT('',#7187);
#2023=VERTEX_POINT('',#7189);
#2024=VERTEX_POINT('',#7191);
#2025=VERTEX_POINT('',#7195);
#2026=VERTEX_POINT('',#7197);
#2027=VERTEX_POINT('',#7201);
#2028=VERTEX_POINT('',#7202);
#2029=VERTEX_POINT('',#7204);
#2030=VERTEX_POINT('',#7206);
#2031=VERTEX_POINT('',#7210);
#2032=VERTEX_POINT('',#7212);
#2033=VERTEX_POINT('',#7216);
#2034=VERTEX_POINT('',#7217);
#2035=VERTEX_POINT('',#7219);
#2036=VERTEX_POINT('',#7221);
#2037=VERTEX_POINT('',#7225);
#2038=VERTEX_POINT('',#7227);
#2039=VERTEX_POINT('',#7231);
#2040=VERTEX_POINT('',#7232);
#2041=VERTEX_POINT('',#7234);
#2042=VERTEX_POINT('',#7236);
#2043=VERTEX_POINT('',#7240);
#2044=VERTEX_POINT('',#7242);
#2045=VERTEX_POINT('',#7246);
#2046=VERTEX_POINT('',#7247);
#2047=VERTEX_POINT('',#7249);
#2048=VERTEX_POINT('',#7251);
#2049=VERTEX_POINT('',#7255);
#2050=VERTEX_POINT('',#7257);
#2051=VERTEX_POINT('',#7261);
#2052=VERTEX_POINT('',#7262);
#2053=VERTEX_POINT('',#7264);
#2054=VERTEX_POINT('',#7266);
#2055=VERTEX_POINT('',#7270);
#2056=VERTEX_POINT('',#7272);
#2057=VERTEX_POINT('',#7276);
#2058=VERTEX_POINT('',#7277);
#2059=VERTEX_POINT('',#7279);
#2060=VERTEX_POINT('',#7281);
#2061=VERTEX_POINT('',#7285);
#2062=VERTEX_POINT('',#7287);
#2063=VERTEX_POINT('',#7291);
#2064=VERTEX_POINT('',#7292);
#2065=VERTEX_POINT('',#7294);
#2066=VERTEX_POINT('',#7296);
#2067=VERTEX_POINT('',#7300);
#2068=VERTEX_POINT('',#7302);
#2069=VERTEX_POINT('',#7306);
#2070=VERTEX_POINT('',#7307);
#2071=VERTEX_POINT('',#7309);
#2072=VERTEX_POINT('',#7311);
#2073=VERTEX_POINT('',#7315);
#2074=VERTEX_POINT('',#7317);
#2075=VERTEX_POINT('',#7321);
#2076=VERTEX_POINT('',#7322);
#2077=VERTEX_POINT('',#7324);
#2078=VERTEX_POINT('',#7326);
#2079=VERTEX_POINT('',#7330);
#2080=VERTEX_POINT('',#7332);
#2081=VERTEX_POINT('',#7336);
#2082=VERTEX_POINT('',#7337);
#2083=VERTEX_POINT('',#7339);
#2084=VERTEX_POINT('',#7341);
#2085=VERTEX_POINT('',#7345);
#2086=VERTEX_POINT('',#7347);
#2087=VERTEX_POINT('',#7351);
#2088=VERTEX_POINT('',#7352);
#2089=VERTEX_POINT('',#7354);
#2090=VERTEX_POINT('',#7356);
#2091=VERTEX_POINT('',#7360);
#2092=VERTEX_POINT('',#7362);
#2093=VERTEX_POINT('',#7366);
#2094=VERTEX_POINT('',#7367);
#2095=VERTEX_POINT('',#7369);
#2096=VERTEX_POINT('',#7371);
#2097=VERTEX_POINT('',#7375);
#2098=VERTEX_POINT('',#7377);
#2099=VERTEX_POINT('',#7381);
#2100=VERTEX_POINT('',#7382);
#2101=VERTEX_POINT('',#7384);
#2102=VERTEX_POINT('',#7386);
#2103=VERTEX_POINT('',#7390);
#2104=VERTEX_POINT('',#7392);
#2105=VERTEX_POINT('',#7545);
#2106=VERTEX_POINT('',#7620);
#2107=VERTEX_POINT('',#7690);
#2108=VERTEX_POINT('',#7692);
#2109=VERTEX_POINT('',#8139);
#2110=VERTEX_POINT('',#8214);
#2111=VERTEX_POINT('',#8284);
#2112=VERTEX_POINT('',#8286);
#2113=VERTEX_POINT('',#8739);
#2114=VERTEX_POINT('',#8814);
#2115=VERTEX_POINT('',#8884);
#2116=VERTEX_POINT('',#8886);
#2117=VERTEX_POINT('',#9333);
#2118=VERTEX_POINT('',#9408);
#2119=VERTEX_POINT('',#9478);
#2120=VERTEX_POINT('',#9480);
#2121=VERTEX_POINT('',#9927);
#2122=VERTEX_POINT('',#10002);
#2123=VERTEX_POINT('',#10072);
#2124=VERTEX_POINT('',#10074);
#2125=VERTEX_POINT('',#10521);
#2126=VERTEX_POINT('',#10596);
#2127=VERTEX_POINT('',#10666);
#2128=VERTEX_POINT('',#10668);
#2129=VERTEX_POINT('',#11115);
#2130=VERTEX_POINT('',#11190);
#2131=VERTEX_POINT('',#11260);
#2132=VERTEX_POINT('',#11262);
#2133=VERTEX_POINT('',#11709);
#2134=VERTEX_POINT('',#11784);
#2135=VERTEX_POINT('',#11854);
#2136=VERTEX_POINT('',#11856);
#2137=VERTEX_POINT('',#12303);
#2138=VERTEX_POINT('',#12378);
#2139=VERTEX_POINT('',#12448);
#2140=VERTEX_POINT('',#12450);
#2141=VERTEX_POINT('',#12897);
#2142=VERTEX_POINT('',#12972);
#2143=VERTEX_POINT('',#13042);
#2144=VERTEX_POINT('',#13044);
#2145=VERTEX_POINT('',#13491);
#2146=VERTEX_POINT('',#13566);
#2147=VERTEX_POINT('',#13636);
#2148=VERTEX_POINT('',#13638);
#2149=VERTEX_POINT('',#14085);
#2150=VERTEX_POINT('',#14160);
#2151=VERTEX_POINT('',#14230);
#2152=VERTEX_POINT('',#14232);
#2153=VERTEX_POINT('',#14679);
#2154=VERTEX_POINT('',#14754);
#2155=VERTEX_POINT('',#14824);
#2156=VERTEX_POINT('',#14826);
#2157=VERTEX_POINT('',#15273);
#2158=VERTEX_POINT('',#15348);
#2159=VERTEX_POINT('',#15418);
#2160=VERTEX_POINT('',#15420);
#2161=VERTEX_POINT('',#15867);
#2162=VERTEX_POINT('',#15942);
#2163=VERTEX_POINT('',#16012);
#2164=VERTEX_POINT('',#16014);
#2165=VERTEX_POINT('',#16461);
#2166=VERTEX_POINT('',#16536);
#2167=VERTEX_POINT('',#16606);
#2168=VERTEX_POINT('',#16608);
#2169=VERTEX_POINT('',#17055);
#2170=VERTEX_POINT('',#17130);
#2171=VERTEX_POINT('',#17215);
#2172=VERTEX_POINT('',#17217);
#2173=VERTEX_POINT('',#17664);
#2174=VERTEX_POINT('',#17739);
#2175=VERTEX_POINT('',#17809);
#2176=VERTEX_POINT('',#17811);
#2177=VERTEX_POINT('',#18258);
#2178=VERTEX_POINT('',#18333);
#2179=VERTEX_POINT('',#18403);
#2180=VERTEX_POINT('',#18405);
#2181=VERTEX_POINT('',#18720);
#2182=VERTEX_POINT('',#18722);
#2183=VERTEX_POINT('',#18724);
#2184=VERTEX_POINT('',#18726);
#2185=VERTEX_POINT('',#18801);
#2186=VERTEX_POINT('',#18803);
#2187=VERTEX_POINT('',#18878);
#2188=VERTEX_POINT('',#18880);
#2189=VERTEX_POINT('',#18885);
#2190=VERTEX_POINT('',#18887);
#2191=VERTEX_POINT('',#18889);
#2192=VERTEX_POINT('',#18891);
#2193=VERTEX_POINT('',#18962);
#2194=VERTEX_POINT('',#18964);
#2195=VERTEX_POINT('',#19032);
#2196=VERTEX_POINT('',#19034);
#2197=VERTEX_POINT('',#19390);
#2198=VERTEX_POINT('',#19392);
#2199=VERTEX_POINT('',#19396);
#2200=VERTEX_POINT('',#19398);
#2201=VERTEX_POINT('',#19402);
#2202=VERTEX_POINT('',#19408);
#2203=VERTEX_POINT('',#19409);
#2204=VERTEX_POINT('',#19411);
#2205=VERTEX_POINT('',#19415);
#2206=VERTEX_POINT('',#19419);
#2207=VERTEX_POINT('',#19423);
#2208=VERTEX_POINT('',#19427);
#2209=VERTEX_POINT('',#19433);
#2210=VERTEX_POINT('',#19434);
#2211=VERTEX_POINT('',#19439);
#2212=VERTEX_POINT('',#19443);
#2213=VERTEX_POINT('',#19447);
#2214=VERTEX_POINT('',#19451);
#2215=VERTEX_POINT('',#19457);
#2216=VERTEX_POINT('',#19464);
#2217=VERTEX_POINT('',#19466);
#2218=VERTEX_POINT('',#19470);
#2219=VERTEX_POINT('',#19472);
#2220=VERTEX_POINT('',#19476);
#2221=VERTEX_POINT('',#19482);
#2222=VERTEX_POINT('',#19483);
#2223=VERTEX_POINT('',#19485);
#2224=VERTEX_POINT('',#19489);
#2225=VERTEX_POINT('',#19493);
#2226=VERTEX_POINT('',#19497);
#2227=VERTEX_POINT('',#19501);
#2228=VERTEX_POINT('',#19507);
#2229=VERTEX_POINT('',#19508);
#2230=VERTEX_POINT('',#19513);
#2231=VERTEX_POINT('',#19517);
#2232=VERTEX_POINT('',#19521);
#2233=VERTEX_POINT('',#19525);
#2234=VERTEX_POINT('',#19531);
#2235=VERTEX_POINT('',#19538);
#2236=VERTEX_POINT('',#19540);
#2237=VERTEX_POINT('',#19544);
#2238=VERTEX_POINT('',#19547);
#2239=VERTEX_POINT('',#19549);
#2240=VERTEX_POINT('',#19555);
#2241=VERTEX_POINT('',#19558);
#2242=VERTEX_POINT('',#19565);
#2243=VERTEX_POINT('',#19567);
#2244=VERTEX_POINT('',#19571);
#2245=VERTEX_POINT('',#19575);
#2246=VERTEX_POINT('',#19578);
#2247=VERTEX_POINT('',#19580);
#2248=VERTEX_POINT('',#19584);
#2249=VERTEX_POINT('',#19587);
#2250=VERTEX_POINT('',#19591);
#2251=VERTEX_POINT('',#19595);
#2252=VERTEX_POINT('',#19600);
#2253=VERTEX_POINT('',#19604);
#2254=VERTEX_POINT('',#19608);
#2255=VERTEX_POINT('',#19611);
#2256=VERTEX_POINT('',#19615);
#2257=VERTEX_POINT('',#19618);
#2258=VERTEX_POINT('',#19622);
#2259=VERTEX_POINT('',#19625);
#2260=VERTEX_POINT('',#19631);
#2261=VERTEX_POINT('',#19632);
#2262=VERTEX_POINT('',#19634);
#2263=VERTEX_POINT('',#19636);
#2264=VERTEX_POINT('',#19640);
#2265=VERTEX_POINT('',#19641);
#2266=VERTEX_POINT('',#19644);
#2267=VERTEX_POINT('',#19650);
#2268=VERTEX_POINT('',#19652);
#2269=VERTEX_POINT('',#19654);
#2270=VERTEX_POINT('',#19660);
#2271=VERTEX_POINT('',#19662);
#2272=VERTEX_POINT('',#19664);
#2273=VERTEX_POINT('',#19666);
#2274=VERTEX_POINT('',#19670);
#2275=VERTEX_POINT('',#19674);
#2276=VERTEX_POINT('',#19676);
#2277=VERTEX_POINT('',#19678);
#2278=VERTEX_POINT('',#19681);
#2279=VERTEX_POINT('',#19684);
#2280=VERTEX_POINT('',#19688);
#2281=VERTEX_POINT('',#19690);
#2282=VERTEX_POINT('',#19692);
#2283=VERTEX_POINT('',#19696);
#2284=VERTEX_POINT('',#19700);
#2285=VERTEX_POINT('',#19706);
#2286=VERTEX_POINT('',#19710);
#2287=VERTEX_POINT('',#19714);
#2288=VERTEX_POINT('',#19718);
#2289=VERTEX_POINT('',#19726);
#2290=VERTEX_POINT('',#19728);
#2291=VERTEX_POINT('',#19732);
#2292=VERTEX_POINT('',#19734);
#2293=VERTEX_POINT('',#19738);
#2294=VERTEX_POINT('',#19739);
#2295=VERTEX_POINT('',#19741);
#2296=VERTEX_POINT('',#19743);
#2297=VERTEX_POINT('',#19747);
#2298=VERTEX_POINT('',#19748);
#2299=VERTEX_POINT('',#19750);
#2300=VERTEX_POINT('',#19757);
#2301=VERTEX_POINT('',#19759);
#2302=VERTEX_POINT('',#19761);
#2303=VERTEX_POINT('',#19768);
#2304=VERTEX_POINT('',#19770);
#2305=VERTEX_POINT('',#19774);
#2306=VERTEX_POINT('',#19778);
#2307=VERTEX_POINT('',#19780);
#2308=VERTEX_POINT('',#19782);
#2309=VERTEX_POINT('',#19785);
#2310=VERTEX_POINT('',#19788);
#2311=VERTEX_POINT('',#19793);
#2312=VERTEX_POINT('',#19797);
#2313=VERTEX_POINT('',#19801);
#2314=VERTEX_POINT('',#19807);
#2315=VERTEX_POINT('',#19811);
#2316=VERTEX_POINT('',#19815);
#2317=VERTEX_POINT('',#19819);
#2318=VERTEX_POINT('',#19827);
#2319=VERTEX_POINT('',#19829);
#2320=VERTEX_POINT('',#19835);
#2321=VERTEX_POINT('',#19838);
#2322=VERTEX_POINT('',#19842);
#2323=VERTEX_POINT('',#19845);
#2324=VERTEX_POINT('',#19851);
#2325=EDGE_CURVE('',#1875,#1875,#1609,.T.);
#2326=EDGE_CURVE('',#1875,#1876,#897,.T.);
#2327=EDGE_CURVE('',#1876,#1876,#1610,.T.);
#2328=EDGE_CURVE('',#1877,#1878,#1611,.F.);
#2329=EDGE_CURVE('',#1878,#1879,#898,.T.);
#2330=EDGE_CURVE('',#1879,#1880,#1612,.T.);
#2331=EDGE_CURVE('',#1880,#1877,#899,.T.);
#2332=EDGE_CURVE('',#1881,#1878,#900,.T.);
#2333=EDGE_CURVE('',#1882,#1881,#901,.T.);
#2334=EDGE_CURVE('',#1879,#1882,#902,.T.);
#2335=EDGE_CURVE('',#1883,#1884,#1613,.T.);
#2336=EDGE_CURVE('',#1884,#1885,#903,.T.);
#2337=EDGE_CURVE('',#1885,#1886,#1614,.F.);
#2338=EDGE_CURVE('',#1886,#1883,#904,.T.);
#2339=EDGE_CURVE('',#1884,#1887,#905,.T.);
#2340=EDGE_CURVE('',#1887,#1888,#906,.T.);
#2341=EDGE_CURVE('',#1885,#1888,#907,.T.);
#2342=EDGE_CURVE('',#1889,#1890,#1615,.F.);
#2343=EDGE_CURVE('',#1890,#1891,#908,.T.);
#2344=EDGE_CURVE('',#1891,#1892,#1616,.T.);
#2345=EDGE_CURVE('',#1892,#1889,#909,.T.);
#2346=EDGE_CURVE('',#1893,#1890,#910,.T.);
#2347=EDGE_CURVE('',#1894,#1893,#911,.T.);
#2348=EDGE_CURVE('',#1891,#1894,#912,.T.);
#2349=EDGE_CURVE('',#1895,#1896,#1617,.T.);
#2350=EDGE_CURVE('',#1896,#1897,#913,.T.);
#2351=EDGE_CURVE('',#1897,#1898,#1618,.F.);
#2352=EDGE_CURVE('',#1898,#1895,#914,.T.);
#2353=EDGE_CURVE('',#1896,#1899,#915,.T.);
#2354=EDGE_CURVE('',#1899,#1900,#916,.T.);
#2355=EDGE_CURVE('',#1897,#1900,#917,.T.);
#2356=EDGE_CURVE('',#1901,#1902,#1619,.F.);
#2357=EDGE_CURVE('',#1902,#1903,#918,.T.);
#2358=EDGE_CURVE('',#1903,#1904,#1620,.T.);
#2359=EDGE_CURVE('',#1904,#1901,#919,.T.);
#2360=EDGE_CURVE('',#1905,#1902,#920,.T.);
#2361=EDGE_CURVE('',#1906,#1905,#921,.T.);
#2362=EDGE_CURVE('',#1903,#1906,#922,.T.);
#2363=EDGE_CURVE('',#1907,#1908,#1621,.T.);
#2364=EDGE_CURVE('',#1908,#1909,#923,.T.);
#2365=EDGE_CURVE('',#1909,#1910,#1622,.F.);
#2366=EDGE_CURVE('',#1910,#1907,#924,.T.);
#2367=EDGE_CURVE('',#1908,#1911,#925,.T.);
#2368=EDGE_CURVE('',#1911,#1912,#926,.T.);
#2369=EDGE_CURVE('',#1909,#1912,#927,.T.);
#2370=EDGE_CURVE('',#1913,#1914,#1623,.F.);
#2371=EDGE_CURVE('',#1914,#1915,#928,.T.);
#2372=EDGE_CURVE('',#1915,#1916,#1624,.T.);
#2373=EDGE_CURVE('',#1916,#1913,#929,.T.);
#2374=EDGE_CURVE('',#1917,#1914,#930,.T.);
#2375=EDGE_CURVE('',#1918,#1917,#931,.T.);
#2376=EDGE_CURVE('',#1915,#1918,#932,.T.);
#2377=EDGE_CURVE('',#1919,#1920,#1625,.T.);
#2378=EDGE_CURVE('',#1920,#1921,#933,.T.);
#2379=EDGE_CURVE('',#1921,#1922,#1626,.F.);
#2380=EDGE_CURVE('',#1922,#1919,#934,.T.);
#2381=EDGE_CURVE('',#1920,#1923,#935,.T.);
#2382=EDGE_CURVE('',#1923,#1924,#936,.T.);
#2383=EDGE_CURVE('',#1921,#1924,#937,.T.);
#2384=EDGE_CURVE('',#1925,#1926,#1627,.F.);
#2385=EDGE_CURVE('',#1926,#1927,#938,.T.);
#2386=EDGE_CURVE('',#1927,#1928,#1628,.T.);
#2387=EDGE_CURVE('',#1928,#1925,#939,.T.);
#2388=EDGE_CURVE('',#1929,#1926,#940,.T.);
#2389=EDGE_CURVE('',#1930,#1929,#941,.T.);
#2390=EDGE_CURVE('',#1927,#1930,#942,.T.);
#2391=EDGE_CURVE('',#1931,#1932,#1629,.T.);
#2392=EDGE_CURVE('',#1932,#1933,#943,.T.);
#2393=EDGE_CURVE('',#1933,#1934,#1630,.F.);
#2394=EDGE_CURVE('',#1934,#1931,#944,.T.);
#2395=EDGE_CURVE('',#1932,#1935,#945,.T.);
#2396=EDGE_CURVE('',#1935,#1936,#946,.T.);
#2397=EDGE_CURVE('',#1933,#1936,#947,.T.);
#2398=EDGE_CURVE('',#1937,#1938,#1631,.F.);
#2399=EDGE_CURVE('',#1938,#1939,#948,.T.);
#2400=EDGE_CURVE('',#1939,#1940,#1632,.T.);
#2401=EDGE_CURVE('',#1940,#1937,#949,.T.);
#2402=EDGE_CURVE('',#1941,#1938,#950,.T.);
#2403=EDGE_CURVE('',#1942,#1941,#951,.T.);
#2404=EDGE_CURVE('',#1939,#1942,#952,.T.);
#2405=EDGE_CURVE('',#1943,#1944,#1633,.T.);
#2406=EDGE_CURVE('',#1944,#1945,#953,.T.);
#2407=EDGE_CURVE('',#1945,#1946,#1634,.F.);
#2408=EDGE_CURVE('',#1946,#1943,#954,.T.);
#2409=EDGE_CURVE('',#1944,#1947,#955,.T.);
#2410=EDGE_CURVE('',#1947,#1948,#956,.T.);
#2411=EDGE_CURVE('',#1945,#1948,#957,.T.);
#2412=EDGE_CURVE('',#1949,#1950,#1635,.F.);
#2413=EDGE_CURVE('',#1950,#1951,#958,.T.);
#2414=EDGE_CURVE('',#1951,#1952,#1636,.T.);
#2415=EDGE_CURVE('',#1952,#1949,#959,.T.);
#2416=EDGE_CURVE('',#1953,#1950,#960,.T.);
#2417=EDGE_CURVE('',#1954,#1953,#961,.T.);
#2418=EDGE_CURVE('',#1951,#1954,#962,.T.);
#2419=EDGE_CURVE('',#1955,#1956,#1637,.T.);
#2420=EDGE_CURVE('',#1956,#1957,#963,.T.);
#2421=EDGE_CURVE('',#1957,#1958,#1638,.F.);
#2422=EDGE_CURVE('',#1958,#1955,#964,.T.);
#2423=EDGE_CURVE('',#1956,#1959,#965,.T.);
#2424=EDGE_CURVE('',#1959,#1960,#966,.T.);
#2425=EDGE_CURVE('',#1957,#1960,#967,.T.);
#2426=EDGE_CURVE('',#1961,#1962,#1639,.F.);
#2427=EDGE_CURVE('',#1962,#1963,#968,.T.);
#2428=EDGE_CURVE('',#1963,#1964,#1640,.T.);
#2429=EDGE_CURVE('',#1964,#1961,#969,.T.);
#2430=EDGE_CURVE('',#1965,#1962,#970,.T.);
#2431=EDGE_CURVE('',#1966,#1965,#971,.T.);
#2432=EDGE_CURVE('',#1963,#1966,#972,.T.);
#2433=EDGE_CURVE('',#1967,#1968,#1641,.T.);
#2434=EDGE_CURVE('',#1968,#1969,#973,.T.);
#2435=EDGE_CURVE('',#1969,#1970,#1642,.F.);
#2436=EDGE_CURVE('',#1970,#1967,#974,.T.);
#2437=EDGE_CURVE('',#1968,#1971,#975,.T.);
#2438=EDGE_CURVE('',#1971,#1972,#976,.T.);
#2439=EDGE_CURVE('',#1969,#1972,#977,.T.);
#2440=EDGE_CURVE('',#1973,#1974,#1643,.F.);
#2441=EDGE_CURVE('',#1974,#1975,#978,.T.);
#2442=EDGE_CURVE('',#1975,#1976,#1644,.T.);
#2443=EDGE_CURVE('',#1976,#1973,#979,.T.);
#2444=EDGE_CURVE('',#1977,#1974,#980,.T.);
#2445=EDGE_CURVE('',#1978,#1977,#981,.T.);
#2446=EDGE_CURVE('',#1975,#1978,#982,.T.);
#2447=EDGE_CURVE('',#1979,#1980,#1645,.T.);
#2448=EDGE_CURVE('',#1980,#1981,#983,.T.);
#2449=EDGE_CURVE('',#1981,#1982,#1646,.F.);
#2450=EDGE_CURVE('',#1982,#1979,#984,.T.);
#2451=EDGE_CURVE('',#1980,#1983,#985,.T.);
#2452=EDGE_CURVE('',#1983,#1984,#986,.T.);
#2453=EDGE_CURVE('',#1981,#1984,#987,.T.);
#2454=EDGE_CURVE('',#1985,#1986,#1647,.F.);
#2455=EDGE_CURVE('',#1986,#1987,#988,.T.);
#2456=EDGE_CURVE('',#1987,#1988,#1648,.T.);
#2457=EDGE_CURVE('',#1988,#1985,#989,.T.);
#2458=EDGE_CURVE('',#1989,#1986,#990,.T.);
#2459=EDGE_CURVE('',#1990,#1989,#991,.T.);
#2460=EDGE_CURVE('',#1987,#1990,#992,.T.);
#2461=EDGE_CURVE('',#1991,#1992,#1649,.T.);
#2462=EDGE_CURVE('',#1992,#1993,#993,.T.);
#2463=EDGE_CURVE('',#1993,#1994,#1650,.F.);
#2464=EDGE_CURVE('',#1994,#1991,#994,.T.);
#2465=EDGE_CURVE('',#1992,#1995,#995,.T.);
#2466=EDGE_CURVE('',#1995,#1996,#996,.T.);
#2467=EDGE_CURVE('',#1993,#1996,#997,.T.);
#2468=EDGE_CURVE('',#1997,#1998,#1651,.F.);
#2469=EDGE_CURVE('',#1998,#1999,#998,.T.);
#2470=EDGE_CURVE('',#1999,#2000,#1652,.T.);
#2471=EDGE_CURVE('',#2000,#1997,#999,.T.);
#2472=EDGE_CURVE('',#2001,#1998,#1000,.T.);
#2473=EDGE_CURVE('',#2002,#2001,#1001,.T.);
#2474=EDGE_CURVE('',#1999,#2002,#1002,.T.);
#2475=EDGE_CURVE('',#2003,#2004,#1653,.T.);
#2476=EDGE_CURVE('',#2004,#2005,#1003,.T.);
#2477=EDGE_CURVE('',#2005,#2006,#1654,.F.);
#2478=EDGE_CURVE('',#2006,#2003,#1004,.T.);
#2479=EDGE_CURVE('',#2004,#2007,#1005,.T.);
#2480=EDGE_CURVE('',#2007,#2008,#1006,.T.);
#2481=EDGE_CURVE('',#2005,#2008,#1007,.T.);
#2482=EDGE_CURVE('',#2009,#2010,#1655,.F.);
#2483=EDGE_CURVE('',#2010,#2011,#1008,.T.);
#2484=EDGE_CURVE('',#2011,#2012,#1656,.T.);
#2485=EDGE_CURVE('',#2012,#2009,#1009,.T.);
#2486=EDGE_CURVE('',#2013,#2010,#1010,.T.);
#2487=EDGE_CURVE('',#2014,#2013,#1011,.T.);
#2488=EDGE_CURVE('',#2011,#2014,#1012,.T.);
#2489=EDGE_CURVE('',#2015,#2016,#1657,.T.);
#2490=EDGE_CURVE('',#2016,#2017,#1013,.T.);
#2491=EDGE_CURVE('',#2017,#2018,#1658,.F.);
#2492=EDGE_CURVE('',#2018,#2015,#1014,.T.);
#2493=EDGE_CURVE('',#2016,#2019,#1015,.T.);
#2494=EDGE_CURVE('',#2019,#2020,#1016,.T.);
#2495=EDGE_CURVE('',#2017,#2020,#1017,.T.);
#2496=EDGE_CURVE('',#2021,#2022,#1659,.F.);
#2497=EDGE_CURVE('',#2022,#2023,#1018,.T.);
#2498=EDGE_CURVE('',#2023,#2024,#1660,.T.);
#2499=EDGE_CURVE('',#2024,#2021,#1019,.T.);
#2500=EDGE_CURVE('',#2025,#2022,#1020,.T.);
#2501=EDGE_CURVE('',#2026,#2025,#1021,.T.);
#2502=EDGE_CURVE('',#2023,#2026,#1022,.T.);
#2503=EDGE_CURVE('',#2027,#2028,#1661,.T.);
#2504=EDGE_CURVE('',#2028,#2029,#1023,.T.);
#2505=EDGE_CURVE('',#2029,#2030,#1662,.F.);
#2506=EDGE_CURVE('',#2030,#2027,#1024,.T.);
#2507=EDGE_CURVE('',#2028,#2031,#1025,.T.);
#2508=EDGE_CURVE('',#2031,#2032,#1026,.T.);
#2509=EDGE_CURVE('',#2029,#2032,#1027,.T.);
#2510=EDGE_CURVE('',#2033,#2034,#1663,.F.);
#2511=EDGE_CURVE('',#2034,#2035,#1028,.T.);
#2512=EDGE_CURVE('',#2035,#2036,#1664,.T.);
#2513=EDGE_CURVE('',#2036,#2033,#1029,.T.);
#2514=EDGE_CURVE('',#2037,#2034,#1030,.T.);
#2515=EDGE_CURVE('',#2038,#2037,#1031,.T.);
#2516=EDGE_CURVE('',#2035,#2038,#1032,.T.);
#2517=EDGE_CURVE('',#2039,#2040,#1665,.T.);
#2518=EDGE_CURVE('',#2040,#2041,#1033,.T.);
#2519=EDGE_CURVE('',#2041,#2042,#1666,.F.);
#2520=EDGE_CURVE('',#2042,#2039,#1034,.T.);
#2521=EDGE_CURVE('',#2040,#2043,#1035,.T.);
#2522=EDGE_CURVE('',#2043,#2044,#1036,.T.);
#2523=EDGE_CURVE('',#2041,#2044,#1037,.T.);
#2524=EDGE_CURVE('',#2045,#2046,#1667,.F.);
#2525=EDGE_CURVE('',#2046,#2047,#1038,.T.);
#2526=EDGE_CURVE('',#2047,#2048,#1668,.T.);
#2527=EDGE_CURVE('',#2048,#2045,#1039,.T.);
#2528=EDGE_CURVE('',#2049,#2046,#1040,.T.);
#2529=EDGE_CURVE('',#2050,#2049,#1041,.T.);
#2530=EDGE_CURVE('',#2047,#2050,#1042,.T.);
#2531=EDGE_CURVE('',#2051,#2052,#1669,.T.);
#2532=EDGE_CURVE('',#2052,#2053,#1043,.T.);
#2533=EDGE_CURVE('',#2053,#2054,#1670,.F.);
#2534=EDGE_CURVE('',#2054,#2051,#1044,.T.);
#2535=EDGE_CURVE('',#2052,#2055,#1045,.T.);
#2536=EDGE_CURVE('',#2055,#2056,#1046,.T.);
#2537=EDGE_CURVE('',#2053,#2056,#1047,.T.);
#2538=EDGE_CURVE('',#2057,#2058,#1671,.F.);
#2539=EDGE_CURVE('',#2058,#2059,#1048,.T.);
#2540=EDGE_CURVE('',#2059,#2060,#1672,.T.);
#2541=EDGE_CURVE('',#2060,#2057,#1049,.T.);
#2542=EDGE_CURVE('',#2061,#2058,#1050,.T.);
#2543=EDGE_CURVE('',#2062,#2061,#1051,.T.);
#2544=EDGE_CURVE('',#2059,#2062,#1052,.T.);
#2545=EDGE_CURVE('',#2063,#2064,#1673,.T.);
#2546=EDGE_CURVE('',#2064,#2065,#1053,.T.);
#2547=EDGE_CURVE('',#2065,#2066,#1674,.F.);
#2548=EDGE_CURVE('',#2066,#2063,#1054,.T.);
#2549=EDGE_CURVE('',#2064,#2067,#1055,.T.);
#2550=EDGE_CURVE('',#2067,#2068,#1056,.T.);
#2551=EDGE_CURVE('',#2065,#2068,#1057,.T.);
#2552=EDGE_CURVE('',#2069,#2070,#1675,.F.);
#2553=EDGE_CURVE('',#2070,#2071,#1058,.T.);
#2554=EDGE_CURVE('',#2071,#2072,#1676,.T.);
#2555=EDGE_CURVE('',#2072,#2069,#1059,.T.);
#2556=EDGE_CURVE('',#2073,#2070,#1060,.T.);
#2557=EDGE_CURVE('',#2074,#2073,#1061,.T.);
#2558=EDGE_CURVE('',#2071,#2074,#1062,.T.);
#2559=EDGE_CURVE('',#2075,#2076,#1677,.T.);
#2560=EDGE_CURVE('',#2076,#2077,#1063,.T.);
#2561=EDGE_CURVE('',#2077,#2078,#1678,.F.);
#2562=EDGE_CURVE('',#2078,#2075,#1064,.T.);
#2563=EDGE_CURVE('',#2076,#2079,#1065,.T.);
#2564=EDGE_CURVE('',#2079,#2080,#1066,.T.);
#2565=EDGE_CURVE('',#2077,#2080,#1067,.T.);
#2566=EDGE_CURVE('',#2081,#2082,#1679,.F.);
#2567=EDGE_CURVE('',#2082,#2083,#1068,.T.);
#2568=EDGE_CURVE('',#2083,#2084,#1680,.T.);
#2569=EDGE_CURVE('',#2084,#2081,#1069,.T.);
#2570=EDGE_CURVE('',#2085,#2082,#1070,.T.);
#2571=EDGE_CURVE('',#2086,#2085,#1071,.T.);
#2572=EDGE_CURVE('',#2083,#2086,#1072,.T.);
#2573=EDGE_CURVE('',#2087,#2088,#1681,.T.);
#2574=EDGE_CURVE('',#2088,#2089,#1073,.T.);
#2575=EDGE_CURVE('',#2089,#2090,#1682,.F.);
#2576=EDGE_CURVE('',#2090,#2087,#1074,.T.);
#2577=EDGE_CURVE('',#2088,#2091,#1075,.T.);
#2578=EDGE_CURVE('',#2091,#2092,#1076,.T.);
#2579=EDGE_CURVE('',#2089,#2092,#1077,.T.);
#2580=EDGE_CURVE('',#2093,#2094,#1683,.F.);
#2581=EDGE_CURVE('',#2094,#2095,#1078,.T.);
#2582=EDGE_CURVE('',#2095,#2096,#1684,.T.);
#2583=EDGE_CURVE('',#2096,#2093,#1079,.T.);
#2584=EDGE_CURVE('',#2097,#2094,#1080,.T.);
#2585=EDGE_CURVE('',#2098,#2097,#1081,.T.);
#2586=EDGE_CURVE('',#2095,#2098,#1082,.T.);
#2587=EDGE_CURVE('',#2099,#2100,#1685,.T.);
#2588=EDGE_CURVE('',#2100,#2101,#1083,.T.);
#2589=EDGE_CURVE('',#2101,#2102,#1686,.F.);
#2590=EDGE_CURVE('',#2102,#2099,#1084,.T.);
#2591=EDGE_CURVE('',#2100,#2103,#1085,.T.);
#2592=EDGE_CURVE('',#2103,#2104,#1086,.T.);
#2593=EDGE_CURVE('',#2101,#2104,#1087,.T.);
#2594=EDGE_CURVE('',#1882,#2105,#111,.T.);
#2595=EDGE_CURVE('',#2106,#1881,#112,.T.);
#2596=EDGE_CURVE('',#2105,#2106,#1088,.T.);
#2597=EDGE_CURVE('',#2107,#2105,#1687,.T.);
#2598=EDGE_CURVE('',#2108,#2106,#1688,.T.);
#2599=EDGE_CURVE('',#2107,#2108,#1089,.T.);
#2600=EDGE_CURVE('',#1887,#2107,#113,.T.);
#2601=EDGE_CURVE('',#1888,#2108,#114,.T.);
#2602=EDGE_CURVE('',#1894,#2109,#115,.T.);
#2603=EDGE_CURVE('',#2110,#1893,#116,.T.);
#2604=EDGE_CURVE('',#2109,#2110,#1090,.T.);
#2605=EDGE_CURVE('',#2111,#2109,#1689,.T.);
#2606=EDGE_CURVE('',#2112,#2110,#1690,.T.);
#2607=EDGE_CURVE('',#2111,#2112,#1091,.T.);
#2608=EDGE_CURVE('',#1899,#2111,#117,.T.);
#2609=EDGE_CURVE('',#1900,#2112,#118,.T.);
#2610=EDGE_CURVE('',#1906,#2113,#119,.T.);
#2611=EDGE_CURVE('',#2114,#1905,#120,.T.);
#2612=EDGE_CURVE('',#2113,#2114,#1092,.T.);
#2613=EDGE_CURVE('',#2115,#2113,#1691,.T.);
#2614=EDGE_CURVE('',#2116,#2114,#1692,.T.);
#2615=EDGE_CURVE('',#2115,#2116,#1093,.T.);
#2616=EDGE_CURVE('',#1911,#2115,#121,.T.);
#2617=EDGE_CURVE('',#1912,#2116,#122,.T.);
#2618=EDGE_CURVE('',#1918,#2117,#123,.T.);
#2619=EDGE_CURVE('',#2118,#1917,#124,.T.);
#2620=EDGE_CURVE('',#2117,#2118,#1094,.T.);
#2621=EDGE_CURVE('',#2119,#2117,#1693,.T.);
#2622=EDGE_CURVE('',#2120,#2118,#1694,.T.);
#2623=EDGE_CURVE('',#2119,#2120,#1095,.T.);
#2624=EDGE_CURVE('',#1923,#2119,#125,.T.);
#2625=EDGE_CURVE('',#1924,#2120,#126,.T.);
#2626=EDGE_CURVE('',#1930,#2121,#127,.T.);
#2627=EDGE_CURVE('',#2122,#1929,#128,.T.);
#2628=EDGE_CURVE('',#2121,#2122,#1096,.T.);
#2629=EDGE_CURVE('',#2123,#2121,#1695,.T.);
#2630=EDGE_CURVE('',#2124,#2122,#1696,.T.);
#2631=EDGE_CURVE('',#2123,#2124,#1097,.T.);
#2632=EDGE_CURVE('',#1935,#2123,#129,.T.);
#2633=EDGE_CURVE('',#1936,#2124,#130,.T.);
#2634=EDGE_CURVE('',#1942,#2125,#131,.T.);
#2635=EDGE_CURVE('',#2126,#1941,#132,.T.);
#2636=EDGE_CURVE('',#2125,#2126,#1098,.T.);
#2637=EDGE_CURVE('',#2127,#2125,#1697,.T.);
#2638=EDGE_CURVE('',#2128,#2126,#1698,.T.);
#2639=EDGE_CURVE('',#2127,#2128,#1099,.T.);
#2640=EDGE_CURVE('',#1947,#2127,#133,.T.);
#2641=EDGE_CURVE('',#1948,#2128,#134,.T.);
#2642=EDGE_CURVE('',#1954,#2129,#135,.T.);
#2643=EDGE_CURVE('',#2130,#1953,#136,.T.);
#2644=EDGE_CURVE('',#2129,#2130,#1100,.T.);
#2645=EDGE_CURVE('',#2131,#2129,#1699,.T.);
#2646=EDGE_CURVE('',#2132,#2130,#1700,.T.);
#2647=EDGE_CURVE('',#2131,#2132,#1101,.T.);
#2648=EDGE_CURVE('',#1959,#2131,#137,.T.);
#2649=EDGE_CURVE('',#1960,#2132,#138,.T.);
#2650=EDGE_CURVE('',#1966,#2133,#139,.T.);
#2651=EDGE_CURVE('',#2134,#1965,#140,.T.);
#2652=EDGE_CURVE('',#2133,#2134,#1102,.T.);
#2653=EDGE_CURVE('',#2135,#2133,#1701,.T.);
#2654=EDGE_CURVE('',#2136,#2134,#1702,.T.);
#2655=EDGE_CURVE('',#2135,#2136,#1103,.T.);
#2656=EDGE_CURVE('',#1971,#2135,#141,.T.);
#2657=EDGE_CURVE('',#1972,#2136,#142,.T.);
#2658=EDGE_CURVE('',#1978,#2137,#143,.T.);
#2659=EDGE_CURVE('',#2138,#1977,#144,.T.);
#2660=EDGE_CURVE('',#2137,#2138,#1104,.T.);
#2661=EDGE_CURVE('',#2139,#2137,#1703,.T.);
#2662=EDGE_CURVE('',#2140,#2138,#1704,.T.);
#2663=EDGE_CURVE('',#2139,#2140,#1105,.T.);
#2664=EDGE_CURVE('',#1983,#2139,#145,.T.);
#2665=EDGE_CURVE('',#1984,#2140,#146,.T.);
#2666=EDGE_CURVE('',#1990,#2141,#147,.T.);
#2667=EDGE_CURVE('',#2142,#1989,#148,.T.);
#2668=EDGE_CURVE('',#2141,#2142,#1106,.T.);
#2669=EDGE_CURVE('',#2143,#2141,#1705,.T.);
#2670=EDGE_CURVE('',#2144,#2142,#1706,.T.);
#2671=EDGE_CURVE('',#2143,#2144,#1107,.T.);
#2672=EDGE_CURVE('',#1995,#2143,#149,.T.);
#2673=EDGE_CURVE('',#1996,#2144,#150,.T.);
#2674=EDGE_CURVE('',#2002,#2145,#151,.T.);
#2675=EDGE_CURVE('',#2146,#2001,#152,.T.);
#2676=EDGE_CURVE('',#2145,#2146,#1108,.T.);
#2677=EDGE_CURVE('',#2147,#2145,#1707,.T.);
#2678=EDGE_CURVE('',#2148,#2146,#1708,.T.);
#2679=EDGE_CURVE('',#2147,#2148,#1109,.T.);
#2680=EDGE_CURVE('',#2007,#2147,#153,.T.);
#2681=EDGE_CURVE('',#2008,#2148,#154,.T.);
#2682=EDGE_CURVE('',#2014,#2149,#155,.T.);
#2683=EDGE_CURVE('',#2150,#2013,#156,.T.);
#2684=EDGE_CURVE('',#2149,#2150,#1110,.T.);
#2685=EDGE_CURVE('',#2151,#2149,#1709,.T.);
#2686=EDGE_CURVE('',#2152,#2150,#1710,.T.);
#2687=EDGE_CURVE('',#2151,#2152,#1111,.T.);
#2688=EDGE_CURVE('',#2019,#2151,#157,.T.);
#2689=EDGE_CURVE('',#2020,#2152,#158,.T.);
#2690=EDGE_CURVE('',#2026,#2153,#159,.T.);
#2691=EDGE_CURVE('',#2154,#2025,#160,.T.);
#2692=EDGE_CURVE('',#2153,#2154,#1112,.T.);
#2693=EDGE_CURVE('',#2155,#2153,#1711,.T.);
#2694=EDGE_CURVE('',#2156,#2154,#1712,.T.);
#2695=EDGE_CURVE('',#2155,#2156,#1113,.T.);
#2696=EDGE_CURVE('',#2031,#2155,#161,.T.);
#2697=EDGE_CURVE('',#2032,#2156,#162,.T.);
#2698=EDGE_CURVE('',#2038,#2157,#163,.T.);
#2699=EDGE_CURVE('',#2158,#2037,#164,.T.);
#2700=EDGE_CURVE('',#2157,#2158,#1114,.T.);
#2701=EDGE_CURVE('',#2159,#2157,#1713,.T.);
#2702=EDGE_CURVE('',#2160,#2158,#1714,.T.);
#2703=EDGE_CURVE('',#2159,#2160,#1115,.T.);
#2704=EDGE_CURVE('',#2043,#2159,#165,.T.);
#2705=EDGE_CURVE('',#2044,#2160,#166,.T.);
#2706=EDGE_CURVE('',#2050,#2161,#167,.T.);
#2707=EDGE_CURVE('',#2162,#2049,#168,.T.);
#2708=EDGE_CURVE('',#2161,#2162,#1116,.T.);
#2709=EDGE_CURVE('',#2163,#2161,#1715,.T.);
#2710=EDGE_CURVE('',#2164,#2162,#1716,.T.);
#2711=EDGE_CURVE('',#2163,#2164,#1117,.T.);
#2712=EDGE_CURVE('',#2055,#2163,#169,.T.);
#2713=EDGE_CURVE('',#2056,#2164,#170,.T.);
#2714=EDGE_CURVE('',#2062,#2165,#171,.T.);
#2715=EDGE_CURVE('',#2166,#2061,#172,.T.);
#2716=EDGE_CURVE('',#2165,#2166,#1118,.T.);
#2717=EDGE_CURVE('',#2167,#2165,#1717,.T.);
#2718=EDGE_CURVE('',#2168,#2166,#1718,.T.);
#2719=EDGE_CURVE('',#2167,#2168,#1119,.T.);
#2720=EDGE_CURVE('',#2067,#2167,#173,.T.);
#2721=EDGE_CURVE('',#2068,#2168,#174,.T.);
#2722=EDGE_CURVE('',#2074,#2169,#175,.T.);
#2723=EDGE_CURVE('',#2170,#2073,#176,.T.);
#2724=EDGE_CURVE('',#2169,#2170,#1120,.T.);
#2725=EDGE_CURVE('',#2171,#2169,#1719,.T.);
#2726=EDGE_CURVE('',#2172,#2170,#1720,.T.);
#2727=EDGE_CURVE('',#2171,#2172,#1121,.T.);
#2728=EDGE_CURVE('',#2079,#2171,#177,.T.);
#2729=EDGE_CURVE('',#2080,#2172,#178,.T.);
#2730=EDGE_CURVE('',#2086,#2173,#179,.T.);
#2731=EDGE_CURVE('',#2174,#2085,#180,.T.);
#2732=EDGE_CURVE('',#2173,#2174,#1122,.T.);
#2733=EDGE_CURVE('',#2175,#2173,#1721,.T.);
#2734=EDGE_CURVE('',#2176,#2174,#1722,.T.);
#2735=EDGE_CURVE('',#2175,#2176,#1123,.T.);
#2736=EDGE_CURVE('',#2091,#2175,#181,.T.);
#2737=EDGE_CURVE('',#2092,#2176,#182,.T.);
#2738=EDGE_CURVE('',#2098,#2177,#183,.T.);
#2739=EDGE_CURVE('',#2178,#2097,#184,.T.);
#2740=EDGE_CURVE('',#2177,#2178,#1124,.T.);
#2741=EDGE_CURVE('',#2179,#2177,#1723,.T.);
#2742=EDGE_CURVE('',#2180,#2178,#1724,.T.);
#2743=EDGE_CURVE('',#2179,#2180,#1125,.T.);
#2744=EDGE_CURVE('',#2103,#2179,#185,.T.);
#2745=EDGE_CURVE('',#2104,#2180,#186,.T.);
#2746=EDGE_CURVE('',#1904,#1895,#1725,.T.);
#2747=EDGE_CURVE('',#1916,#1907,#1726,.T.);
#2748=EDGE_CURVE('',#1928,#1919,#1727,.T.);
#2749=EDGE_CURVE('',#1940,#1931,#1728,.T.);
#2750=EDGE_CURVE('',#1952,#1943,#1729,.T.);
#2751=EDGE_CURVE('',#1964,#1955,#1730,.T.);
#2752=EDGE_CURVE('',#1976,#1967,#1731,.T.);
#2753=EDGE_CURVE('',#1988,#1979,#1732,.T.);
#2754=EDGE_CURVE('',#2000,#1991,#1733,.T.);
#2755=EDGE_CURVE('',#2012,#2003,#1734,.T.);
#2756=EDGE_CURVE('',#2024,#2015,#1735,.T.);
#2757=EDGE_CURVE('',#2036,#2027,#1736,.T.);
#2758=EDGE_CURVE('',#2048,#2039,#1737,.T.);
#2759=EDGE_CURVE('',#2060,#2051,#1738,.T.);
#2760=EDGE_CURVE('',#2072,#2063,#1739,.T.);
#2761=EDGE_CURVE('',#2084,#2075,#1740,.T.);
#2762=EDGE_CURVE('',#2096,#2087,#1741,.T.);
#2763=EDGE_CURVE('',#2181,#2099,#1742,.T.);
#2764=EDGE_CURVE('',#2182,#2181,#1743,.T.);
#2765=EDGE_CURVE('',#2182,#2183,#1126,.T.);
#2766=EDGE_CURVE('',#2183,#2184,#187,.T.);
#2767=EDGE_CURVE('',#2185,#2184,#1744,.T.);
#2768=EDGE_CURVE('',#2186,#2185,#188,.T.);
#2769=EDGE_CURVE('',#2187,#2186,#1127,.T.);
#2770=EDGE_CURVE('',#2188,#2187,#1745,.T.);
#2771=EDGE_CURVE('',#1880,#2188,#1746,.T.);
#2772=EDGE_CURVE('',#1892,#1883,#1747,.T.);
#2773=EDGE_CURVE('',#1877,#2189,#1748,.T.);
#2774=EDGE_CURVE('',#2190,#2189,#1749,.F.);
#2775=EDGE_CURVE('',#2190,#2191,#1128,.T.);
#2776=EDGE_CURVE('',#2191,#2192,#189,.T.);
#2777=EDGE_CURVE('',#2192,#2193,#1750,.T.);
#2778=EDGE_CURVE('',#2193,#2194,#190,.T.);
#2779=EDGE_CURVE('',#2194,#2195,#1129,.T.);
#2780=EDGE_CURVE('',#2196,#2195,#1751,.F.);
#2781=EDGE_CURVE('',#2196,#2102,#1752,.T.);
#2782=EDGE_CURVE('',#2093,#2090,#1753,.T.);
#2783=EDGE_CURVE('',#2081,#2078,#1754,.T.);
#2784=EDGE_CURVE('',#2069,#2066,#1755,.T.);
#2785=EDGE_CURVE('',#2057,#2054,#1756,.T.);
#2786=EDGE_CURVE('',#2045,#2042,#1757,.T.);
#2787=EDGE_CURVE('',#2033,#2030,#1758,.T.);
#2788=EDGE_CURVE('',#2021,#2018,#1759,.T.);
#2789=EDGE_CURVE('',#2009,#2006,#1760,.T.);
#2790=EDGE_CURVE('',#1997,#1994,#1761,.T.);
#2791=EDGE_CURVE('',#1985,#1982,#1762,.T.);
#2792=EDGE_CURVE('',#1973,#1970,#1763,.T.);
#2793=EDGE_CURVE('',#1961,#1958,#1764,.T.);
#2794=EDGE_CURVE('',#1949,#1946,#1765,.T.);
#2795=EDGE_CURVE('',#1937,#1934,#1766,.T.);
#2796=EDGE_CURVE('',#1925,#1922,#1767,.T.);
#2797=EDGE_CURVE('',#1913,#1910,#1768,.T.);
#2798=EDGE_CURVE('',#1901,#1898,#1769,.T.);
#2799=EDGE_CURVE('',#1889,#1886,#1770,.T.);
#2800=EDGE_CURVE('',#2181,#2196,#1130,.T.);
#2801=EDGE_CURVE('',#2195,#2182,#1131,.T.);
#2802=EDGE_CURVE('',#2183,#2194,#1132,.T.);
#2803=EDGE_CURVE('',#2187,#2190,#1133,.T.);
#2804=EDGE_CURVE('',#2189,#2188,#1134,.T.);
#2805=EDGE_CURVE('',#2186,#2191,#1135,.T.);
#2806=EDGE_CURVE('',#2184,#2193,#1136,.T.);
#2807=EDGE_CURVE('',#2185,#2192,#1137,.T.);
#2808=EDGE_CURVE('',#2197,#2197,#1771,.T.);
#2809=EDGE_CURVE('',#2197,#2198,#1138,.T.);
#2810=EDGE_CURVE('',#2198,#2198,#1772,.T.);
#2811=EDGE_CURVE('',#2199,#2199,#1773,.T.);
#2812=EDGE_CURVE('',#2199,#2200,#1774,.T.);
#2813=EDGE_CURVE('',#2200,#2200,#1775,.T.);
#2814=EDGE_CURVE('',#2201,#2201,#1776,.T.);
#2815=EDGE_CURVE('',#2201,#2200,#1139,.T.);
#2816=EDGE_CURVE('',#2197,#2199,#1140,.T.);
#2817=EDGE_CURVE('',#2202,#2203,#1141,.T.);
#2818=EDGE_CURVE('',#2204,#2202,#1142,.T.);
#2819=EDGE_CURVE('',#2204,#2203,#1143,.T.);
#2820=EDGE_CURVE('',#2205,#2204,#1144,.T.);
#2821=EDGE_CURVE('',#2205,#2203,#1145,.T.);
#2822=EDGE_CURVE('',#2206,#2205,#1146,.T.);
#2823=EDGE_CURVE('',#2206,#2203,#1147,.T.);
#2824=EDGE_CURVE('',#2207,#2206,#1148,.T.);
#2825=EDGE_CURVE('',#2207,#2203,#1149,.T.);
#2826=EDGE_CURVE('',#2208,#2207,#1150,.T.);
#2827=EDGE_CURVE('',#2208,#2203,#1151,.T.);
#2828=EDGE_CURVE('',#2202,#2208,#1152,.T.);
#2829=EDGE_CURVE('',#2209,#2210,#1153,.T.);
#2830=EDGE_CURVE('',#2209,#2204,#1154,.T.);
#2831=EDGE_CURVE('',#2210,#2202,#1155,.T.);
#2832=EDGE_CURVE('',#2211,#2209,#1156,.T.);
#2833=EDGE_CURVE('',#2211,#2205,#1157,.T.);
#2834=EDGE_CURVE('',#2212,#2211,#1158,.T.);
#2835=EDGE_CURVE('',#2212,#2206,#1159,.T.);
#2836=EDGE_CURVE('',#2213,#2212,#1160,.T.);
#2837=EDGE_CURVE('',#2213,#2207,#1161,.T.);
#2838=EDGE_CURVE('',#2214,#2213,#1162,.T.);
#2839=EDGE_CURVE('',#2214,#2208,#1163,.T.);
#2840=EDGE_CURVE('',#2210,#2214,#1164,.T.);
#2841=EDGE_CURVE('',#2215,#2215,#1777,.T.);
#2842=EDGE_CURVE('',#2201,#2215,#1165,.T.);
#2843=EDGE_CURVE('',#2216,#2216,#1778,.T.);
#2844=EDGE_CURVE('',#2216,#2217,#1166,.T.);
#2845=EDGE_CURVE('',#2217,#2217,#1779,.T.);
#2846=EDGE_CURVE('',#2218,#2218,#1780,.T.);
#2847=EDGE_CURVE('',#2218,#2219,#1781,.T.);
#2848=EDGE_CURVE('',#2219,#2219,#1782,.T.);
#2849=EDGE_CURVE('',#2220,#2220,#1783,.T.);
#2850=EDGE_CURVE('',#2220,#2219,#1167,.T.);
#2851=EDGE_CURVE('',#2216,#2218,#1168,.T.);
#2852=EDGE_CURVE('',#2221,#2222,#1169,.T.);
#2853=EDGE_CURVE('',#2223,#2221,#1170,.T.);
#2854=EDGE_CURVE('',#2223,#2222,#1171,.T.);
#2855=EDGE_CURVE('',#2224,#2223,#1172,.T.);
#2856=EDGE_CURVE('',#2224,#2222,#1173,.T.);
#2857=EDGE_CURVE('',#2225,#2224,#1174,.T.);
#2858=EDGE_CURVE('',#2225,#2222,#1175,.T.);
#2859=EDGE_CURVE('',#2226,#2225,#1176,.T.);
#2860=EDGE_CURVE('',#2226,#2222,#1177,.T.);
#2861=EDGE_CURVE('',#2227,#2226,#1178,.T.);
#2862=EDGE_CURVE('',#2227,#2222,#1179,.T.);
#2863=EDGE_CURVE('',#2221,#2227,#1180,.T.);
#2864=EDGE_CURVE('',#2228,#2229,#1181,.T.);
#2865=EDGE_CURVE('',#2228,#2223,#1182,.T.);
#2866=EDGE_CURVE('',#2229,#2221,#1183,.T.);
#2867=EDGE_CURVE('',#2230,#2228,#1184,.T.);
#2868=EDGE_CURVE('',#2230,#2224,#1185,.T.);
#2869=EDGE_CURVE('',#2231,#2230,#1186,.T.);
#2870=EDGE_CURVE('',#2231,#2225,#1187,.T.);
#2871=EDGE_CURVE('',#2232,#2231,#1188,.T.);
#2872=EDGE_CURVE('',#2232,#2226,#1189,.T.);
#2873=EDGE_CURVE('',#2233,#2232,#1190,.T.);
#2874=EDGE_CURVE('',#2233,#2227,#1191,.T.);
#2875=EDGE_CURVE('',#2229,#2233,#1192,.T.);
#2876=EDGE_CURVE('',#2234,#2234,#1784,.T.);
#2877=EDGE_CURVE('',#2220,#2234,#1193,.T.);
#2878=EDGE_CURVE('',#2235,#2235,#1785,.T.);
#2879=EDGE_CURVE('',#2235,#2236,#1194,.T.);
#2880=EDGE_CURVE('',#2236,#2236,#1786,.T.);
#2881=EDGE_CURVE('',#2237,#2237,#1787,.T.);
#2882=EDGE_CURVE('',#2238,#2238,#1788,.T.);
#2883=EDGE_CURVE('',#2238,#2239,#1789,.T.);
#2884=EDGE_CURVE('',#2239,#2239,#1790,.T.);
#2885=EDGE_CURVE('',#2237,#2238,#1195,.T.);
#2886=EDGE_CURVE('',#2240,#2240,#1791,.T.);
#2887=EDGE_CURVE('',#2241,#2241,#1792,.T.);
#2888=EDGE_CURVE('',#2241,#2240,#1196,.T.);
#2889=EDGE_CURVE('',#2242,#2242,#1793,.T.);
#2890=EDGE_CURVE('',#2242,#2243,#1794,.T.);
#2891=EDGE_CURVE('',#2243,#2243,#1795,.T.);
#2892=EDGE_CURVE('',#2243,#2244,#1197,.T.);
#2893=EDGE_CURVE('',#2244,#2244,#1796,.T.);
#2894=EDGE_CURVE('',#2245,#2245,#1797,.T.);
#2895=EDGE_CURVE('',#2246,#2246,#1798,.T.);
#2896=EDGE_CURVE('',#2246,#2247,#1799,.T.);
#2897=EDGE_CURVE('',#2247,#2247,#1800,.T.);
#2898=EDGE_CURVE('',#2248,#2248,#1801,.T.);
#2899=EDGE_CURVE('',#2249,#2249,#1802,.T.);
#2900=EDGE_CURVE('',#2249,#2246,#1198,.T.);
#2901=EDGE_CURVE('',#2248,#2250,#1803,.T.);
#2902=EDGE_CURVE('',#2250,#2250,#1804,.T.);
#2903=EDGE_CURVE('',#2250,#2251,#1199,.T.);
#2904=EDGE_CURVE('',#2251,#2251,#1805,.T.);
#2905=EDGE_CURVE('',#2252,#2252,#1806,.T.);
#2906=EDGE_CURVE('',#2252,#2245,#1200,.T.);
#2907=EDGE_CURVE('',#2253,#2253,#1807,.T.);
#2908=EDGE_CURVE('',#2253,#2252,#1808,.T.);
#2909=EDGE_CURVE('',#2254,#2254,#1809,.T.);
#2910=EDGE_CURVE('',#2255,#2255,#1810,.T.);
#2911=EDGE_CURVE('',#2255,#2254,#1201,.T.);
#2912=EDGE_CURVE('',#2256,#2256,#1811,.T.);
#2913=EDGE_CURVE('',#2257,#2257,#1812,.T.);
#2914=EDGE_CURVE('',#2257,#2256,#1202,.T.);
#2915=EDGE_CURVE('',#2258,#2258,#1813,.T.);
#2916=EDGE_CURVE('',#2259,#2259,#1814,.T.);
#2917=EDGE_CURVE('',#2259,#2258,#1203,.T.);
#2918=EDGE_CURVE('',#2260,#2261,#1815,.T.);
#2919=EDGE_CURVE('',#2262,#2260,#1204,.T.);
#2920=EDGE_CURVE('',#2263,#2262,#1816,.F.);
#2921=EDGE_CURVE('',#2261,#2263,#1205,.T.);
#2922=EDGE_CURVE('',#2264,#2265,#1817,.T.);
#2923=EDGE_CURVE('',#2260,#2264,#1818,.T.);
#2924=EDGE_CURVE('',#2266,#2260,#1819,.T.);
#2925=EDGE_CURVE('',#2265,#2266,#1820,.T.);
#2926=EDGE_CURVE('',#2266,#2261,#1821,.T.);
#2927=EDGE_CURVE('',#2267,#2264,#1822,.T.);
#2928=EDGE_CURVE('',#2268,#2267,#1206,.T.);
#2929=EDGE_CURVE('',#2269,#2268,#1823,.F.);
#2930=EDGE_CURVE('',#2264,#2269,#1207,.T.);
#2931=EDGE_CURVE('',#2267,#2265,#1824,.T.);
#2932=EDGE_CURVE('',#2270,#2263,#1208,.T.);
#2933=EDGE_CURVE('',#2271,#2270,#1209,.T.);
#2934=EDGE_CURVE('',#2271,#2272,#1210,.T.);
#2935=EDGE_CURVE('',#2272,#2273,#1211,.T.);
#2936=EDGE_CURVE('',#2273,#2261,#1212,.T.);
#2937=EDGE_CURVE('',#2274,#2273,#1825,.T.);
#2938=EDGE_CURVE('',#2266,#2274,#1213,.T.);
#2939=EDGE_CURVE('',#2274,#2275,#1826,.T.);
#2940=EDGE_CURVE('',#2275,#2276,#1214,.T.);
#2941=EDGE_CURVE('',#2276,#2277,#1827,.T.);
#2942=EDGE_CURVE('',#2277,#2265,#1215,.T.);
#2943=EDGE_CURVE('',#2278,#2278,#1828,.T.);
#2944=EDGE_CURVE('',#2277,#2279,#1829,.T.);
#2945=EDGE_CURVE('',#2267,#2279,#1216,.T.);
#2946=EDGE_CURVE('',#2279,#2280,#1217,.T.);
#2947=EDGE_CURVE('',#2280,#2281,#1218,.T.);
#2948=EDGE_CURVE('',#2282,#2281,#1219,.T.);
#2949=EDGE_CURVE('',#2268,#2282,#1220,.T.);
#2950=EDGE_CURVE('',#2275,#2283,#1830,.T.);
#2951=EDGE_CURVE('',#2283,#2273,#1831,.T.);
#2952=EDGE_CURVE('',#2276,#2284,#1832,.T.);
#2953=EDGE_CURVE('',#2284,#2283,#1221,.T.);
#2954=EDGE_CURVE('',#2279,#2284,#1833,.T.);
#2955=EDGE_CURVE('',#2285,#2285,#1834,.T.);
#2956=EDGE_CURVE('',#2285,#2278,#1222,.T.);
#2957=EDGE_CURVE('',#2286,#2286,#1835,.T.);
#2958=EDGE_CURVE('',#2286,#2285,#1223,.T.);
#2959=EDGE_CURVE('',#2287,#2272,#1836,.T.);
#2960=EDGE_CURVE('',#2283,#2287,#1224,.T.);
#2961=EDGE_CURVE('',#2287,#2288,#1225,.T.);
#2962=EDGE_CURVE('',#2288,#2284,#1226,.T.);
#2963=EDGE_CURVE('',#2280,#2288,#1837,.T.);
#2964=EDGE_CURVE('',#2262,#2269,#1838,.T.);
#2965=EDGE_CURVE('',#2281,#2289,#1839,.F.);
#2966=EDGE_CURVE('',#2289,#2290,#1227,.T.);
#2967=EDGE_CURVE('',#2282,#2290,#1840,.T.);
#2968=EDGE_CURVE('',#2291,#2270,#1841,.T.);
#2969=EDGE_CURVE('',#2291,#2292,#1228,.T.);
#2970=EDGE_CURVE('',#2292,#2271,#1842,.F.);
#2971=EDGE_CURVE('',#2293,#2294,#1843,.T.);
#2972=EDGE_CURVE('',#2294,#2295,#1229,.T.);
#2973=EDGE_CURVE('',#2295,#2296,#1844,.F.);
#2974=EDGE_CURVE('',#2296,#2293,#1230,.T.);
#2975=EDGE_CURVE('',#2297,#2298,#1845,.T.);
#2976=EDGE_CURVE('',#2298,#2299,#1846,.T.);
#2977=EDGE_CURVE('',#2299,#2293,#1847,.T.);
#2978=EDGE_CURVE('',#2293,#2297,#1848,.T.);
#2979=EDGE_CURVE('',#2299,#2294,#1849,.T.);
#2980=EDGE_CURVE('',#2300,#2297,#1850,.T.);
#2981=EDGE_CURVE('',#2297,#2301,#1231,.T.);
#2982=EDGE_CURVE('',#2301,#2302,#1851,.F.);
#2983=EDGE_CURVE('',#2302,#2300,#1232,.T.);
#2984=EDGE_CURVE('',#2300,#2298,#1852,.T.);
#2985=EDGE_CURVE('',#2291,#2295,#1233,.T.);
#2986=EDGE_CURVE('',#2303,#2294,#1234,.T.);
#2987=EDGE_CURVE('',#2304,#2303,#1235,.T.);
#2988=EDGE_CURVE('',#2292,#2304,#1236,.T.);
#2989=EDGE_CURVE('',#2299,#2305,#1237,.T.);
#2990=EDGE_CURVE('',#2305,#2303,#1853,.T.);
#2991=EDGE_CURVE('',#2306,#2298,#1238,.T.);
#2992=EDGE_CURVE('',#2307,#2306,#1854,.T.);
#2993=EDGE_CURVE('',#2308,#2307,#1239,.T.);
#2994=EDGE_CURVE('',#2305,#2308,#1855,.T.);
#2995=EDGE_CURVE('',#2309,#2309,#1856,.T.);
#2996=EDGE_CURVE('',#2300,#2310,#1240,.T.);
#2997=EDGE_CURVE('',#2306,#2310,#1857,.T.);
#2998=EDGE_CURVE('',#2302,#2290,#1241,.T.);
#2999=EDGE_CURVE('',#2311,#2289,#1242,.T.);
#3000=EDGE_CURVE('',#2310,#2311,#1243,.T.);
#3001=EDGE_CURVE('',#2308,#2312,#1858,.T.);
#3002=EDGE_CURVE('',#2312,#2303,#1859,.T.);
#3003=EDGE_CURVE('',#2307,#2313,#1860,.T.);
#3004=EDGE_CURVE('',#2313,#2312,#1244,.T.);
#3005=EDGE_CURVE('',#2310,#2313,#1861,.T.);
#3006=EDGE_CURVE('',#2314,#2314,#1862,.T.);
#3007=EDGE_CURVE('',#2314,#2309,#1245,.T.);
#3008=EDGE_CURVE('',#2314,#2315,#1246,.T.);
#3009=EDGE_CURVE('',#2315,#2315,#1863,.T.);
#3010=EDGE_CURVE('',#2312,#2316,#1247,.T.);
#3011=EDGE_CURVE('',#2316,#2304,#1864,.T.);
#3012=EDGE_CURVE('',#2317,#2313,#1248,.T.);
#3013=EDGE_CURVE('',#2316,#2317,#1249,.T.);
#3014=EDGE_CURVE('',#2311,#2317,#1865,.T.);
#3015=EDGE_CURVE('',#2296,#2301,#1866,.T.);
#3016=EDGE_CURVE('',#2318,#2318,#1867,.T.);
#3017=EDGE_CURVE('',#2318,#2319,#1250,.T.);
#3018=EDGE_CURVE('',#2319,#2319,#1868,.T.);
#3019=EDGE_CURVE('',#2320,#2320,#1869,.T.);
#3020=EDGE_CURVE('',#2321,#2321,#1870,.T.);
#3021=EDGE_CURVE('',#2321,#2320,#1251,.T.);
#3022=EDGE_CURVE('',#2322,#2322,#1871,.T.);
#3023=EDGE_CURVE('',#2323,#2323,#1872,.T.);
#3024=EDGE_CURVE('',#2323,#2322,#1252,.T.);
#3025=EDGE_CURVE('',#2324,#2324,#1873,.T.);
#3026=EDGE_CURVE('',#2324,#2324,#1874,.T.);
#3027=ORIENTED_EDGE('',*,*,#2325,.F.);
#3028=ORIENTED_EDGE('',*,*,#2326,.T.);
#3029=ORIENTED_EDGE('',*,*,#2327,.F.);
#3030=ORIENTED_EDGE('',*,*,#2326,.F.);
#3031=ORIENTED_EDGE('',*,*,#2328,.T.);
#3032=ORIENTED_EDGE('',*,*,#2329,.T.);
#3033=ORIENTED_EDGE('',*,*,#2330,.T.);
#3034=ORIENTED_EDGE('',*,*,#2331,.T.);
#3035=ORIENTED_EDGE('',*,*,#2329,.F.);
#3036=ORIENTED_EDGE('',*,*,#2332,.F.);
#3037=ORIENTED_EDGE('',*,*,#2333,.F.);
#3038=ORIENTED_EDGE('',*,*,#2334,.F.);
#3039=ORIENTED_EDGE('',*,*,#2335,.T.);
#3040=ORIENTED_EDGE('',*,*,#2336,.T.);
#3041=ORIENTED_EDGE('',*,*,#2337,.T.);
#3042=ORIENTED_EDGE('',*,*,#2338,.T.);
#3043=ORIENTED_EDGE('',*,*,#2336,.F.);
#3044=ORIENTED_EDGE('',*,*,#2339,.T.);
#3045=ORIENTED_EDGE('',*,*,#2340,.T.);
#3046=ORIENTED_EDGE('',*,*,#2341,.F.);
#3047=ORIENTED_EDGE('',*,*,#2342,.T.);
#3048=ORIENTED_EDGE('',*,*,#2343,.T.);
#3049=ORIENTED_EDGE('',*,*,#2344,.T.);
#3050=ORIENTED_EDGE('',*,*,#2345,.T.);
#3051=ORIENTED_EDGE('',*,*,#2343,.F.);
#3052=ORIENTED_EDGE('',*,*,#2346,.F.);
#3053=ORIENTED_EDGE('',*,*,#2347,.F.);
#3054=ORIENTED_EDGE('',*,*,#2348,.F.);
#3055=ORIENTED_EDGE('',*,*,#2349,.T.);
#3056=ORIENTED_EDGE('',*,*,#2350,.T.);
#3057=ORIENTED_EDGE('',*,*,#2351,.T.);
#3058=ORIENTED_EDGE('',*,*,#2352,.T.);
#3059=ORIENTED_EDGE('',*,*,#2350,.F.);
#3060=ORIENTED_EDGE('',*,*,#2353,.T.);
#3061=ORIENTED_EDGE('',*,*,#2354,.T.);
#3062=ORIENTED_EDGE('',*,*,#2355,.F.);
#3063=ORIENTED_EDGE('',*,*,#2356,.T.);
#3064=ORIENTED_EDGE('',*,*,#2357,.T.);
#3065=ORIENTED_EDGE('',*,*,#2358,.T.);
#3066=ORIENTED_EDGE('',*,*,#2359,.T.);
#3067=ORIENTED_EDGE('',*,*,#2357,.F.);
#3068=ORIENTED_EDGE('',*,*,#2360,.F.);
#3069=ORIENTED_EDGE('',*,*,#2361,.F.);
#3070=ORIENTED_EDGE('',*,*,#2362,.F.);
#3071=ORIENTED_EDGE('',*,*,#2363,.T.);
#3072=ORIENTED_EDGE('',*,*,#2364,.T.);
#3073=ORIENTED_EDGE('',*,*,#2365,.T.);
#3074=ORIENTED_EDGE('',*,*,#2366,.T.);
#3075=ORIENTED_EDGE('',*,*,#2364,.F.);
#3076=ORIENTED_EDGE('',*,*,#2367,.T.);
#3077=ORIENTED_EDGE('',*,*,#2368,.T.);
#3078=ORIENTED_EDGE('',*,*,#2369,.F.);
#3079=ORIENTED_EDGE('',*,*,#2370,.T.);
#3080=ORIENTED_EDGE('',*,*,#2371,.T.);
#3081=ORIENTED_EDGE('',*,*,#2372,.T.);
#3082=ORIENTED_EDGE('',*,*,#2373,.T.);
#3083=ORIENTED_EDGE('',*,*,#2371,.F.);
#3084=ORIENTED_EDGE('',*,*,#2374,.F.);
#3085=ORIENTED_EDGE('',*,*,#2375,.F.);
#3086=ORIENTED_EDGE('',*,*,#2376,.F.);
#3087=ORIENTED_EDGE('',*,*,#2377,.T.);
#3088=ORIENTED_EDGE('',*,*,#2378,.T.);
#3089=ORIENTED_EDGE('',*,*,#2379,.T.);
#3090=ORIENTED_EDGE('',*,*,#2380,.T.);
#3091=ORIENTED_EDGE('',*,*,#2378,.F.);
#3092=ORIENTED_EDGE('',*,*,#2381,.T.);
#3093=ORIENTED_EDGE('',*,*,#2382,.T.);
#3094=ORIENTED_EDGE('',*,*,#2383,.F.);
#3095=ORIENTED_EDGE('',*,*,#2384,.T.);
#3096=ORIENTED_EDGE('',*,*,#2385,.T.);
#3097=ORIENTED_EDGE('',*,*,#2386,.T.);
#3098=ORIENTED_EDGE('',*,*,#2387,.T.);
#3099=ORIENTED_EDGE('',*,*,#2385,.F.);
#3100=ORIENTED_EDGE('',*,*,#2388,.F.);
#3101=ORIENTED_EDGE('',*,*,#2389,.F.);
#3102=ORIENTED_EDGE('',*,*,#2390,.F.);
#3103=ORIENTED_EDGE('',*,*,#2391,.T.);
#3104=ORIENTED_EDGE('',*,*,#2392,.T.);
#3105=ORIENTED_EDGE('',*,*,#2393,.T.);
#3106=ORIENTED_EDGE('',*,*,#2394,.T.);
#3107=ORIENTED_EDGE('',*,*,#2392,.F.);
#3108=ORIENTED_EDGE('',*,*,#2395,.T.);
#3109=ORIENTED_EDGE('',*,*,#2396,.T.);
#3110=ORIENTED_EDGE('',*,*,#2397,.F.);
#3111=ORIENTED_EDGE('',*,*,#2398,.T.);
#3112=ORIENTED_EDGE('',*,*,#2399,.T.);
#3113=ORIENTED_EDGE('',*,*,#2400,.T.);
#3114=ORIENTED_EDGE('',*,*,#2401,.T.);
#3115=ORIENTED_EDGE('',*,*,#2399,.F.);
#3116=ORIENTED_EDGE('',*,*,#2402,.F.);
#3117=ORIENTED_EDGE('',*,*,#2403,.F.);
#3118=ORIENTED_EDGE('',*,*,#2404,.F.);
#3119=ORIENTED_EDGE('',*,*,#2405,.T.);
#3120=ORIENTED_EDGE('',*,*,#2406,.T.);
#3121=ORIENTED_EDGE('',*,*,#2407,.T.);
#3122=ORIENTED_EDGE('',*,*,#2408,.T.);
#3123=ORIENTED_EDGE('',*,*,#2406,.F.);
#3124=ORIENTED_EDGE('',*,*,#2409,.T.);
#3125=ORIENTED_EDGE('',*,*,#2410,.T.);
#3126=ORIENTED_EDGE('',*,*,#2411,.F.);
#3127=ORIENTED_EDGE('',*,*,#2412,.T.);
#3128=ORIENTED_EDGE('',*,*,#2413,.T.);
#3129=ORIENTED_EDGE('',*,*,#2414,.T.);
#3130=ORIENTED_EDGE('',*,*,#2415,.T.);
#3131=ORIENTED_EDGE('',*,*,#2413,.F.);
#3132=ORIENTED_EDGE('',*,*,#2416,.F.);
#3133=ORIENTED_EDGE('',*,*,#2417,.F.);
#3134=ORIENTED_EDGE('',*,*,#2418,.F.);
#3135=ORIENTED_EDGE('',*,*,#2419,.T.);
#3136=ORIENTED_EDGE('',*,*,#2420,.T.);
#3137=ORIENTED_EDGE('',*,*,#2421,.T.);
#3138=ORIENTED_EDGE('',*,*,#2422,.T.);
#3139=ORIENTED_EDGE('',*,*,#2420,.F.);
#3140=ORIENTED_EDGE('',*,*,#2423,.T.);
#3141=ORIENTED_EDGE('',*,*,#2424,.T.);
#3142=ORIENTED_EDGE('',*,*,#2425,.F.);
#3143=ORIENTED_EDGE('',*,*,#2426,.T.);
#3144=ORIENTED_EDGE('',*,*,#2427,.T.);
#3145=ORIENTED_EDGE('',*,*,#2428,.T.);
#3146=ORIENTED_EDGE('',*,*,#2429,.T.);
#3147=ORIENTED_EDGE('',*,*,#2427,.F.);
#3148=ORIENTED_EDGE('',*,*,#2430,.F.);
#3149=ORIENTED_EDGE('',*,*,#2431,.F.);
#3150=ORIENTED_EDGE('',*,*,#2432,.F.);
#3151=ORIENTED_EDGE('',*,*,#2433,.T.);
#3152=ORIENTED_EDGE('',*,*,#2434,.T.);
#3153=ORIENTED_EDGE('',*,*,#2435,.T.);
#3154=ORIENTED_EDGE('',*,*,#2436,.T.);
#3155=ORIENTED_EDGE('',*,*,#2434,.F.);
#3156=ORIENTED_EDGE('',*,*,#2437,.T.);
#3157=ORIENTED_EDGE('',*,*,#2438,.T.);
#3158=ORIENTED_EDGE('',*,*,#2439,.F.);
#3159=ORIENTED_EDGE('',*,*,#2440,.T.);
#3160=ORIENTED_EDGE('',*,*,#2441,.T.);
#3161=ORIENTED_EDGE('',*,*,#2442,.T.);
#3162=ORIENTED_EDGE('',*,*,#2443,.T.);
#3163=ORIENTED_EDGE('',*,*,#2441,.F.);
#3164=ORIENTED_EDGE('',*,*,#2444,.F.);
#3165=ORIENTED_EDGE('',*,*,#2445,.F.);
#3166=ORIENTED_EDGE('',*,*,#2446,.F.);
#3167=ORIENTED_EDGE('',*,*,#2447,.T.);
#3168=ORIENTED_EDGE('',*,*,#2448,.T.);
#3169=ORIENTED_EDGE('',*,*,#2449,.T.);
#3170=ORIENTED_EDGE('',*,*,#2450,.T.);
#3171=ORIENTED_EDGE('',*,*,#2448,.F.);
#3172=ORIENTED_EDGE('',*,*,#2451,.T.);
#3173=ORIENTED_EDGE('',*,*,#2452,.T.);
#3174=ORIENTED_EDGE('',*,*,#2453,.F.);
#3175=ORIENTED_EDGE('',*,*,#2454,.T.);
#3176=ORIENTED_EDGE('',*,*,#2455,.T.);
#3177=ORIENTED_EDGE('',*,*,#2456,.T.);
#3178=ORIENTED_EDGE('',*,*,#2457,.T.);
#3179=ORIENTED_EDGE('',*,*,#2455,.F.);
#3180=ORIENTED_EDGE('',*,*,#2458,.F.);
#3181=ORIENTED_EDGE('',*,*,#2459,.F.);
#3182=ORIENTED_EDGE('',*,*,#2460,.F.);
#3183=ORIENTED_EDGE('',*,*,#2461,.T.);
#3184=ORIENTED_EDGE('',*,*,#2462,.T.);
#3185=ORIENTED_EDGE('',*,*,#2463,.T.);
#3186=ORIENTED_EDGE('',*,*,#2464,.T.);
#3187=ORIENTED_EDGE('',*,*,#2462,.F.);
#3188=ORIENTED_EDGE('',*,*,#2465,.T.);
#3189=ORIENTED_EDGE('',*,*,#2466,.T.);
#3190=ORIENTED_EDGE('',*,*,#2467,.F.);
#3191=ORIENTED_EDGE('',*,*,#2468,.T.);
#3192=ORIENTED_EDGE('',*,*,#2469,.T.);
#3193=ORIENTED_EDGE('',*,*,#2470,.T.);
#3194=ORIENTED_EDGE('',*,*,#2471,.T.);
#3195=ORIENTED_EDGE('',*,*,#2469,.F.);
#3196=ORIENTED_EDGE('',*,*,#2472,.F.);
#3197=ORIENTED_EDGE('',*,*,#2473,.F.);
#3198=ORIENTED_EDGE('',*,*,#2474,.F.);
#3199=ORIENTED_EDGE('',*,*,#2475,.T.);
#3200=ORIENTED_EDGE('',*,*,#2476,.T.);
#3201=ORIENTED_EDGE('',*,*,#2477,.T.);
#3202=ORIENTED_EDGE('',*,*,#2478,.T.);
#3203=ORIENTED_EDGE('',*,*,#2476,.F.);
#3204=ORIENTED_EDGE('',*,*,#2479,.T.);
#3205=ORIENTED_EDGE('',*,*,#2480,.T.);
#3206=ORIENTED_EDGE('',*,*,#2481,.F.);
#3207=ORIENTED_EDGE('',*,*,#2482,.T.);
#3208=ORIENTED_EDGE('',*,*,#2483,.T.);
#3209=ORIENTED_EDGE('',*,*,#2484,.T.);
#3210=ORIENTED_EDGE('',*,*,#2485,.T.);
#3211=ORIENTED_EDGE('',*,*,#2483,.F.);
#3212=ORIENTED_EDGE('',*,*,#2486,.F.);
#3213=ORIENTED_EDGE('',*,*,#2487,.F.);
#3214=ORIENTED_EDGE('',*,*,#2488,.F.);
#3215=ORIENTED_EDGE('',*,*,#2489,.T.);
#3216=ORIENTED_EDGE('',*,*,#2490,.T.);
#3217=ORIENTED_EDGE('',*,*,#2491,.T.);
#3218=ORIENTED_EDGE('',*,*,#2492,.T.);
#3219=ORIENTED_EDGE('',*,*,#2490,.F.);
#3220=ORIENTED_EDGE('',*,*,#2493,.T.);
#3221=ORIENTED_EDGE('',*,*,#2494,.T.);
#3222=ORIENTED_EDGE('',*,*,#2495,.F.);
#3223=ORIENTED_EDGE('',*,*,#2496,.T.);
#3224=ORIENTED_EDGE('',*,*,#2497,.T.);
#3225=ORIENTED_EDGE('',*,*,#2498,.T.);
#3226=ORIENTED_EDGE('',*,*,#2499,.T.);
#3227=ORIENTED_EDGE('',*,*,#2497,.F.);
#3228=ORIENTED_EDGE('',*,*,#2500,.F.);
#3229=ORIENTED_EDGE('',*,*,#2501,.F.);
#3230=ORIENTED_EDGE('',*,*,#2502,.F.);
#3231=ORIENTED_EDGE('',*,*,#2503,.T.);
#3232=ORIENTED_EDGE('',*,*,#2504,.T.);
#3233=ORIENTED_EDGE('',*,*,#2505,.T.);
#3234=ORIENTED_EDGE('',*,*,#2506,.T.);
#3235=ORIENTED_EDGE('',*,*,#2504,.F.);
#3236=ORIENTED_EDGE('',*,*,#2507,.T.);
#3237=ORIENTED_EDGE('',*,*,#2508,.T.);
#3238=ORIENTED_EDGE('',*,*,#2509,.F.);
#3239=ORIENTED_EDGE('',*,*,#2510,.T.);
#3240=ORIENTED_EDGE('',*,*,#2511,.T.);
#3241=ORIENTED_EDGE('',*,*,#2512,.T.);
#3242=ORIENTED_EDGE('',*,*,#2513,.T.);
#3243=ORIENTED_EDGE('',*,*,#2511,.F.);
#3244=ORIENTED_EDGE('',*,*,#2514,.F.);
#3245=ORIENTED_EDGE('',*,*,#2515,.F.);
#3246=ORIENTED_EDGE('',*,*,#2516,.F.);
#3247=ORIENTED_EDGE('',*,*,#2517,.T.);
#3248=ORIENTED_EDGE('',*,*,#2518,.T.);
#3249=ORIENTED_EDGE('',*,*,#2519,.T.);
#3250=ORIENTED_EDGE('',*,*,#2520,.T.);
#3251=ORIENTED_EDGE('',*,*,#2518,.F.);
#3252=ORIENTED_EDGE('',*,*,#2521,.T.);
#3253=ORIENTED_EDGE('',*,*,#2522,.T.);
#3254=ORIENTED_EDGE('',*,*,#2523,.F.);
#3255=ORIENTED_EDGE('',*,*,#2524,.T.);
#3256=ORIENTED_EDGE('',*,*,#2525,.T.);
#3257=ORIENTED_EDGE('',*,*,#2526,.T.);
#3258=ORIENTED_EDGE('',*,*,#2527,.T.);
#3259=ORIENTED_EDGE('',*,*,#2525,.F.);
#3260=ORIENTED_EDGE('',*,*,#2528,.F.);
#3261=ORIENTED_EDGE('',*,*,#2529,.F.);
#3262=ORIENTED_EDGE('',*,*,#2530,.F.);
#3263=ORIENTED_EDGE('',*,*,#2531,.T.);
#3264=ORIENTED_EDGE('',*,*,#2532,.T.);
#3265=ORIENTED_EDGE('',*,*,#2533,.T.);
#3266=ORIENTED_EDGE('',*,*,#2534,.T.);
#3267=ORIENTED_EDGE('',*,*,#2532,.F.);
#3268=ORIENTED_EDGE('',*,*,#2535,.T.);
#3269=ORIENTED_EDGE('',*,*,#2536,.T.);
#3270=ORIENTED_EDGE('',*,*,#2537,.F.);
#3271=ORIENTED_EDGE('',*,*,#2538,.T.);
#3272=ORIENTED_EDGE('',*,*,#2539,.T.);
#3273=ORIENTED_EDGE('',*,*,#2540,.T.);
#3274=ORIENTED_EDGE('',*,*,#2541,.T.);
#3275=ORIENTED_EDGE('',*,*,#2539,.F.);
#3276=ORIENTED_EDGE('',*,*,#2542,.F.);
#3277=ORIENTED_EDGE('',*,*,#2543,.F.);
#3278=ORIENTED_EDGE('',*,*,#2544,.F.);
#3279=ORIENTED_EDGE('',*,*,#2545,.T.);
#3280=ORIENTED_EDGE('',*,*,#2546,.T.);
#3281=ORIENTED_EDGE('',*,*,#2547,.T.);
#3282=ORIENTED_EDGE('',*,*,#2548,.T.);
#3283=ORIENTED_EDGE('',*,*,#2546,.F.);
#3284=ORIENTED_EDGE('',*,*,#2549,.T.);
#3285=ORIENTED_EDGE('',*,*,#2550,.T.);
#3286=ORIENTED_EDGE('',*,*,#2551,.F.);
#3287=ORIENTED_EDGE('',*,*,#2552,.T.);
#3288=ORIENTED_EDGE('',*,*,#2553,.T.);
#3289=ORIENTED_EDGE('',*,*,#2554,.T.);
#3290=ORIENTED_EDGE('',*,*,#2555,.T.);
#3291=ORIENTED_EDGE('',*,*,#2553,.F.);
#3292=ORIENTED_EDGE('',*,*,#2556,.F.);
#3293=ORIENTED_EDGE('',*,*,#2557,.F.);
#3294=ORIENTED_EDGE('',*,*,#2558,.F.);
#3295=ORIENTED_EDGE('',*,*,#2559,.T.);
#3296=ORIENTED_EDGE('',*,*,#2560,.T.);
#3297=ORIENTED_EDGE('',*,*,#2561,.T.);
#3298=ORIENTED_EDGE('',*,*,#2562,.T.);
#3299=ORIENTED_EDGE('',*,*,#2560,.F.);
#3300=ORIENTED_EDGE('',*,*,#2563,.T.);
#3301=ORIENTED_EDGE('',*,*,#2564,.T.);
#3302=ORIENTED_EDGE('',*,*,#2565,.F.);
#3303=ORIENTED_EDGE('',*,*,#2566,.T.);
#3304=ORIENTED_EDGE('',*,*,#2567,.T.);
#3305=ORIENTED_EDGE('',*,*,#2568,.T.);
#3306=ORIENTED_EDGE('',*,*,#2569,.T.);
#3307=ORIENTED_EDGE('',*,*,#2567,.F.);
#3308=ORIENTED_EDGE('',*,*,#2570,.F.);
#3309=ORIENTED_EDGE('',*,*,#2571,.F.);
#3310=ORIENTED_EDGE('',*,*,#2572,.F.);
#3311=ORIENTED_EDGE('',*,*,#2573,.T.);
#3312=ORIENTED_EDGE('',*,*,#2574,.T.);
#3313=ORIENTED_EDGE('',*,*,#2575,.T.);
#3314=ORIENTED_EDGE('',*,*,#2576,.T.);
#3315=ORIENTED_EDGE('',*,*,#2574,.F.);
#3316=ORIENTED_EDGE('',*,*,#2577,.T.);
#3317=ORIENTED_EDGE('',*,*,#2578,.T.);
#3318=ORIENTED_EDGE('',*,*,#2579,.F.);
#3319=ORIENTED_EDGE('',*,*,#2580,.T.);
#3320=ORIENTED_EDGE('',*,*,#2581,.T.);
#3321=ORIENTED_EDGE('',*,*,#2582,.T.);
#3322=ORIENTED_EDGE('',*,*,#2583,.T.);
#3323=ORIENTED_EDGE('',*,*,#2581,.F.);
#3324=ORIENTED_EDGE('',*,*,#2584,.F.);
#3325=ORIENTED_EDGE('',*,*,#2585,.F.);
#3326=ORIENTED_EDGE('',*,*,#2586,.F.);
#3327=ORIENTED_EDGE('',*,*,#2587,.T.);
#3328=ORIENTED_EDGE('',*,*,#2588,.T.);
#3329=ORIENTED_EDGE('',*,*,#2589,.T.);
#3330=ORIENTED_EDGE('',*,*,#2590,.T.);
#3331=ORIENTED_EDGE('',*,*,#2588,.F.);
#3332=ORIENTED_EDGE('',*,*,#2591,.T.);
#3333=ORIENTED_EDGE('',*,*,#2592,.T.);
#3334=ORIENTED_EDGE('',*,*,#2593,.F.);
#3335=ORIENTED_EDGE('',*,*,#2594,.F.);
#3336=ORIENTED_EDGE('',*,*,#2333,.T.);
#3337=ORIENTED_EDGE('',*,*,#2595,.F.);
#3338=ORIENTED_EDGE('',*,*,#2596,.F.);
#3339=ORIENTED_EDGE('',*,*,#2597,.T.);
#3340=ORIENTED_EDGE('',*,*,#2596,.T.);
#3341=ORIENTED_EDGE('',*,*,#2598,.F.);
#3342=ORIENTED_EDGE('',*,*,#2599,.F.);
#3343=ORIENTED_EDGE('',*,*,#2600,.T.);
#3344=ORIENTED_EDGE('',*,*,#2599,.T.);
#3345=ORIENTED_EDGE('',*,*,#2601,.F.);
#3346=ORIENTED_EDGE('',*,*,#2340,.F.);
#3347=ORIENTED_EDGE('',*,*,#2602,.F.);
#3348=ORIENTED_EDGE('',*,*,#2347,.T.);
#3349=ORIENTED_EDGE('',*,*,#2603,.F.);
#3350=ORIENTED_EDGE('',*,*,#2604,.F.);
#3351=ORIENTED_EDGE('',*,*,#2605,.T.);
#3352=ORIENTED_EDGE('',*,*,#2604,.T.);
#3353=ORIENTED_EDGE('',*,*,#2606,.F.);
#3354=ORIENTED_EDGE('',*,*,#2607,.F.);
#3355=ORIENTED_EDGE('',*,*,#2608,.T.);
#3356=ORIENTED_EDGE('',*,*,#2607,.T.);
#3357=ORIENTED_EDGE('',*,*,#2609,.F.);
#3358=ORIENTED_EDGE('',*,*,#2354,.F.);
#3359=ORIENTED_EDGE('',*,*,#2610,.F.);
#3360=ORIENTED_EDGE('',*,*,#2361,.T.);
#3361=ORIENTED_EDGE('',*,*,#2611,.F.);
#3362=ORIENTED_EDGE('',*,*,#2612,.F.);
#3363=ORIENTED_EDGE('',*,*,#2613,.T.);
#3364=ORIENTED_EDGE('',*,*,#2612,.T.);
#3365=ORIENTED_EDGE('',*,*,#2614,.F.);
#3366=ORIENTED_EDGE('',*,*,#2615,.F.);
#3367=ORIENTED_EDGE('',*,*,#2616,.T.);
#3368=ORIENTED_EDGE('',*,*,#2615,.T.);
#3369=ORIENTED_EDGE('',*,*,#2617,.F.);
#3370=ORIENTED_EDGE('',*,*,#2368,.F.);
#3371=ORIENTED_EDGE('',*,*,#2618,.F.);
#3372=ORIENTED_EDGE('',*,*,#2375,.T.);
#3373=ORIENTED_EDGE('',*,*,#2619,.F.);
#3374=ORIENTED_EDGE('',*,*,#2620,.F.);
#3375=ORIENTED_EDGE('',*,*,#2621,.T.);
#3376=ORIENTED_EDGE('',*,*,#2620,.T.);
#3377=ORIENTED_EDGE('',*,*,#2622,.F.);
#3378=ORIENTED_EDGE('',*,*,#2623,.F.);
#3379=ORIENTED_EDGE('',*,*,#2624,.T.);
#3380=ORIENTED_EDGE('',*,*,#2623,.T.);
#3381=ORIENTED_EDGE('',*,*,#2625,.F.);
#3382=ORIENTED_EDGE('',*,*,#2382,.F.);
#3383=ORIENTED_EDGE('',*,*,#2626,.F.);
#3384=ORIENTED_EDGE('',*,*,#2389,.T.);
#3385=ORIENTED_EDGE('',*,*,#2627,.F.);
#3386=ORIENTED_EDGE('',*,*,#2628,.F.);
#3387=ORIENTED_EDGE('',*,*,#2629,.T.);
#3388=ORIENTED_EDGE('',*,*,#2628,.T.);
#3389=ORIENTED_EDGE('',*,*,#2630,.F.);
#3390=ORIENTED_EDGE('',*,*,#2631,.F.);
#3391=ORIENTED_EDGE('',*,*,#2632,.T.);
#3392=ORIENTED_EDGE('',*,*,#2631,.T.);
#3393=ORIENTED_EDGE('',*,*,#2633,.F.);
#3394=ORIENTED_EDGE('',*,*,#2396,.F.);
#3395=ORIENTED_EDGE('',*,*,#2634,.F.);
#3396=ORIENTED_EDGE('',*,*,#2403,.T.);
#3397=ORIENTED_EDGE('',*,*,#2635,.F.);
#3398=ORIENTED_EDGE('',*,*,#2636,.F.);
#3399=ORIENTED_EDGE('',*,*,#2637,.T.);
#3400=ORIENTED_EDGE('',*,*,#2636,.T.);
#3401=ORIENTED_EDGE('',*,*,#2638,.F.);
#3402=ORIENTED_EDGE('',*,*,#2639,.F.);
#3403=ORIENTED_EDGE('',*,*,#2640,.T.);
#3404=ORIENTED_EDGE('',*,*,#2639,.T.);
#3405=ORIENTED_EDGE('',*,*,#2641,.F.);
#3406=ORIENTED_EDGE('',*,*,#2410,.F.);
#3407=ORIENTED_EDGE('',*,*,#2642,.F.);
#3408=ORIENTED_EDGE('',*,*,#2417,.T.);
#3409=ORIENTED_EDGE('',*,*,#2643,.F.);
#3410=ORIENTED_EDGE('',*,*,#2644,.F.);
#3411=ORIENTED_EDGE('',*,*,#2645,.T.);
#3412=ORIENTED_EDGE('',*,*,#2644,.T.);
#3413=ORIENTED_EDGE('',*,*,#2646,.F.);
#3414=ORIENTED_EDGE('',*,*,#2647,.F.);
#3415=ORIENTED_EDGE('',*,*,#2648,.T.);
#3416=ORIENTED_EDGE('',*,*,#2647,.T.);
#3417=ORIENTED_EDGE('',*,*,#2649,.F.);
#3418=ORIENTED_EDGE('',*,*,#2424,.F.);
#3419=ORIENTED_EDGE('',*,*,#2650,.F.);
#3420=ORIENTED_EDGE('',*,*,#2431,.T.);
#3421=ORIENTED_EDGE('',*,*,#2651,.F.);
#3422=ORIENTED_EDGE('',*,*,#2652,.F.);
#3423=ORIENTED_EDGE('',*,*,#2653,.T.);
#3424=ORIENTED_EDGE('',*,*,#2652,.T.);
#3425=ORIENTED_EDGE('',*,*,#2654,.F.);
#3426=ORIENTED_EDGE('',*,*,#2655,.F.);
#3427=ORIENTED_EDGE('',*,*,#2656,.T.);
#3428=ORIENTED_EDGE('',*,*,#2655,.T.);
#3429=ORIENTED_EDGE('',*,*,#2657,.F.);
#3430=ORIENTED_EDGE('',*,*,#2438,.F.);
#3431=ORIENTED_EDGE('',*,*,#2658,.F.);
#3432=ORIENTED_EDGE('',*,*,#2445,.T.);
#3433=ORIENTED_EDGE('',*,*,#2659,.F.);
#3434=ORIENTED_EDGE('',*,*,#2660,.F.);
#3435=ORIENTED_EDGE('',*,*,#2661,.T.);
#3436=ORIENTED_EDGE('',*,*,#2660,.T.);
#3437=ORIENTED_EDGE('',*,*,#2662,.F.);
#3438=ORIENTED_EDGE('',*,*,#2663,.F.);
#3439=ORIENTED_EDGE('',*,*,#2664,.T.);
#3440=ORIENTED_EDGE('',*,*,#2663,.T.);
#3441=ORIENTED_EDGE('',*,*,#2665,.F.);
#3442=ORIENTED_EDGE('',*,*,#2452,.F.);
#3443=ORIENTED_EDGE('',*,*,#2666,.F.);
#3444=ORIENTED_EDGE('',*,*,#2459,.T.);
#3445=ORIENTED_EDGE('',*,*,#2667,.F.);
#3446=ORIENTED_EDGE('',*,*,#2668,.F.);
#3447=ORIENTED_EDGE('',*,*,#2669,.T.);
#3448=ORIENTED_EDGE('',*,*,#2668,.T.);
#3449=ORIENTED_EDGE('',*,*,#2670,.F.);
#3450=ORIENTED_EDGE('',*,*,#2671,.F.);
#3451=ORIENTED_EDGE('',*,*,#2672,.T.);
#3452=ORIENTED_EDGE('',*,*,#2671,.T.);
#3453=ORIENTED_EDGE('',*,*,#2673,.F.);
#3454=ORIENTED_EDGE('',*,*,#2466,.F.);
#3455=ORIENTED_EDGE('',*,*,#2674,.F.);
#3456=ORIENTED_EDGE('',*,*,#2473,.T.);
#3457=ORIENTED_EDGE('',*,*,#2675,.F.);
#3458=ORIENTED_EDGE('',*,*,#2676,.F.);
#3459=ORIENTED_EDGE('',*,*,#2677,.T.);
#3460=ORIENTED_EDGE('',*,*,#2676,.T.);
#3461=ORIENTED_EDGE('',*,*,#2678,.F.);
#3462=ORIENTED_EDGE('',*,*,#2679,.F.);
#3463=ORIENTED_EDGE('',*,*,#2680,.T.);
#3464=ORIENTED_EDGE('',*,*,#2679,.T.);
#3465=ORIENTED_EDGE('',*,*,#2681,.F.);
#3466=ORIENTED_EDGE('',*,*,#2480,.F.);
#3467=ORIENTED_EDGE('',*,*,#2682,.F.);
#3468=ORIENTED_EDGE('',*,*,#2487,.T.);
#3469=ORIENTED_EDGE('',*,*,#2683,.F.);
#3470=ORIENTED_EDGE('',*,*,#2684,.F.);
#3471=ORIENTED_EDGE('',*,*,#2685,.T.);
#3472=ORIENTED_EDGE('',*,*,#2684,.T.);
#3473=ORIENTED_EDGE('',*,*,#2686,.F.);
#3474=ORIENTED_EDGE('',*,*,#2687,.F.);
#3475=ORIENTED_EDGE('',*,*,#2688,.T.);
#3476=ORIENTED_EDGE('',*,*,#2687,.T.);
#3477=ORIENTED_EDGE('',*,*,#2689,.F.);
#3478=ORIENTED_EDGE('',*,*,#2494,.F.);
#3479=ORIENTED_EDGE('',*,*,#2690,.F.);
#3480=ORIENTED_EDGE('',*,*,#2501,.T.);
#3481=ORIENTED_EDGE('',*,*,#2691,.F.);
#3482=ORIENTED_EDGE('',*,*,#2692,.F.);
#3483=ORIENTED_EDGE('',*,*,#2693,.T.);
#3484=ORIENTED_EDGE('',*,*,#2692,.T.);
#3485=ORIENTED_EDGE('',*,*,#2694,.F.);
#3486=ORIENTED_EDGE('',*,*,#2695,.F.);
#3487=ORIENTED_EDGE('',*,*,#2696,.T.);
#3488=ORIENTED_EDGE('',*,*,#2695,.T.);
#3489=ORIENTED_EDGE('',*,*,#2697,.F.);
#3490=ORIENTED_EDGE('',*,*,#2508,.F.);
#3491=ORIENTED_EDGE('',*,*,#2698,.F.);
#3492=ORIENTED_EDGE('',*,*,#2515,.T.);
#3493=ORIENTED_EDGE('',*,*,#2699,.F.);
#3494=ORIENTED_EDGE('',*,*,#2700,.F.);
#3495=ORIENTED_EDGE('',*,*,#2701,.T.);
#3496=ORIENTED_EDGE('',*,*,#2700,.T.);
#3497=ORIENTED_EDGE('',*,*,#2702,.F.);
#3498=ORIENTED_EDGE('',*,*,#2703,.F.);
#3499=ORIENTED_EDGE('',*,*,#2704,.T.);
#3500=ORIENTED_EDGE('',*,*,#2703,.T.);
#3501=ORIENTED_EDGE('',*,*,#2705,.F.);
#3502=ORIENTED_EDGE('',*,*,#2522,.F.);
#3503=ORIENTED_EDGE('',*,*,#2706,.F.);
#3504=ORIENTED_EDGE('',*,*,#2529,.T.);
#3505=ORIENTED_EDGE('',*,*,#2707,.F.);
#3506=ORIENTED_EDGE('',*,*,#2708,.F.);
#3507=ORIENTED_EDGE('',*,*,#2709,.T.);
#3508=ORIENTED_EDGE('',*,*,#2708,.T.);
#3509=ORIENTED_EDGE('',*,*,#2710,.F.);
#3510=ORIENTED_EDGE('',*,*,#2711,.F.);
#3511=ORIENTED_EDGE('',*,*,#2712,.T.);
#3512=ORIENTED_EDGE('',*,*,#2711,.T.);
#3513=ORIENTED_EDGE('',*,*,#2713,.F.);
#3514=ORIENTED_EDGE('',*,*,#2536,.F.);
#3515=ORIENTED_EDGE('',*,*,#2714,.F.);
#3516=ORIENTED_EDGE('',*,*,#2543,.T.);
#3517=ORIENTED_EDGE('',*,*,#2715,.F.);
#3518=ORIENTED_EDGE('',*,*,#2716,.F.);
#3519=ORIENTED_EDGE('',*,*,#2717,.T.);
#3520=ORIENTED_EDGE('',*,*,#2716,.T.);
#3521=ORIENTED_EDGE('',*,*,#2718,.F.);
#3522=ORIENTED_EDGE('',*,*,#2719,.F.);
#3523=ORIENTED_EDGE('',*,*,#2720,.T.);
#3524=ORIENTED_EDGE('',*,*,#2719,.T.);
#3525=ORIENTED_EDGE('',*,*,#2721,.F.);
#3526=ORIENTED_EDGE('',*,*,#2550,.F.);
#3527=ORIENTED_EDGE('',*,*,#2722,.F.);
#3528=ORIENTED_EDGE('',*,*,#2557,.T.);
#3529=ORIENTED_EDGE('',*,*,#2723,.F.);
#3530=ORIENTED_EDGE('',*,*,#2724,.F.);
#3531=ORIENTED_EDGE('',*,*,#2725,.T.);
#3532=ORIENTED_EDGE('',*,*,#2724,.T.);
#3533=ORIENTED_EDGE('',*,*,#2726,.F.);
#3534=ORIENTED_EDGE('',*,*,#2727,.F.);
#3535=ORIENTED_EDGE('',*,*,#2728,.T.);
#3536=ORIENTED_EDGE('',*,*,#2727,.T.);
#3537=ORIENTED_EDGE('',*,*,#2729,.F.);
#3538=ORIENTED_EDGE('',*,*,#2564,.F.);
#3539=ORIENTED_EDGE('',*,*,#2730,.F.);
#3540=ORIENTED_EDGE('',*,*,#2571,.T.);
#3541=ORIENTED_EDGE('',*,*,#2731,.F.);
#3542=ORIENTED_EDGE('',*,*,#2732,.F.);
#3543=ORIENTED_EDGE('',*,*,#2733,.T.);
#3544=ORIENTED_EDGE('',*,*,#2732,.T.);
#3545=ORIENTED_EDGE('',*,*,#2734,.F.);
#3546=ORIENTED_EDGE('',*,*,#2735,.F.);
#3547=ORIENTED_EDGE('',*,*,#2736,.T.);
#3548=ORIENTED_EDGE('',*,*,#2735,.T.);
#3549=ORIENTED_EDGE('',*,*,#2737,.F.);
#3550=ORIENTED_EDGE('',*,*,#2578,.F.);
#3551=ORIENTED_EDGE('',*,*,#2738,.F.);
#3552=ORIENTED_EDGE('',*,*,#2585,.T.);
#3553=ORIENTED_EDGE('',*,*,#2739,.F.);
#3554=ORIENTED_EDGE('',*,*,#2740,.F.);
#3555=ORIENTED_EDGE('',*,*,#2741,.T.);
#3556=ORIENTED_EDGE('',*,*,#2740,.T.);
#3557=ORIENTED_EDGE('',*,*,#2742,.F.);
#3558=ORIENTED_EDGE('',*,*,#2743,.F.);
#3559=ORIENTED_EDGE('',*,*,#2744,.T.);
#3560=ORIENTED_EDGE('',*,*,#2743,.T.);
#3561=ORIENTED_EDGE('',*,*,#2745,.F.);
#3562=ORIENTED_EDGE('',*,*,#2592,.F.);
#3563=ORIENTED_EDGE('',*,*,#2344,.F.);
#3564=ORIENTED_EDGE('',*,*,#2348,.T.);
#3565=ORIENTED_EDGE('',*,*,#2602,.T.);
#3566=ORIENTED_EDGE('',*,*,#2605,.F.);
#3567=ORIENTED_EDGE('',*,*,#2608,.F.);
#3568=ORIENTED_EDGE('',*,*,#2353,.F.);
#3569=ORIENTED_EDGE('',*,*,#2349,.F.);
#3570=ORIENTED_EDGE('',*,*,#2746,.F.);
#3571=ORIENTED_EDGE('',*,*,#2358,.F.);
#3572=ORIENTED_EDGE('',*,*,#2362,.T.);
#3573=ORIENTED_EDGE('',*,*,#2610,.T.);
#3574=ORIENTED_EDGE('',*,*,#2613,.F.);
#3575=ORIENTED_EDGE('',*,*,#2616,.F.);
#3576=ORIENTED_EDGE('',*,*,#2367,.F.);
#3577=ORIENTED_EDGE('',*,*,#2363,.F.);
#3578=ORIENTED_EDGE('',*,*,#2747,.F.);
#3579=ORIENTED_EDGE('',*,*,#2372,.F.);
#3580=ORIENTED_EDGE('',*,*,#2376,.T.);
#3581=ORIENTED_EDGE('',*,*,#2618,.T.);
#3582=ORIENTED_EDGE('',*,*,#2621,.F.);
#3583=ORIENTED_EDGE('',*,*,#2624,.F.);
#3584=ORIENTED_EDGE('',*,*,#2381,.F.);
#3585=ORIENTED_EDGE('',*,*,#2377,.F.);
#3586=ORIENTED_EDGE('',*,*,#2748,.F.);
#3587=ORIENTED_EDGE('',*,*,#2386,.F.);
#3588=ORIENTED_EDGE('',*,*,#2390,.T.);
#3589=ORIENTED_EDGE('',*,*,#2626,.T.);
#3590=ORIENTED_EDGE('',*,*,#2629,.F.);
#3591=ORIENTED_EDGE('',*,*,#2632,.F.);
#3592=ORIENTED_EDGE('',*,*,#2395,.F.);
#3593=ORIENTED_EDGE('',*,*,#2391,.F.);
#3594=ORIENTED_EDGE('',*,*,#2749,.F.);
#3595=ORIENTED_EDGE('',*,*,#2400,.F.);
#3596=ORIENTED_EDGE('',*,*,#2404,.T.);
#3597=ORIENTED_EDGE('',*,*,#2634,.T.);
#3598=ORIENTED_EDGE('',*,*,#2637,.F.);
#3599=ORIENTED_EDGE('',*,*,#2640,.F.);
#3600=ORIENTED_EDGE('',*,*,#2409,.F.);
#3601=ORIENTED_EDGE('',*,*,#2405,.F.);
#3602=ORIENTED_EDGE('',*,*,#2750,.F.);
#3603=ORIENTED_EDGE('',*,*,#2414,.F.);
#3604=ORIENTED_EDGE('',*,*,#2418,.T.);
#3605=ORIENTED_EDGE('',*,*,#2642,.T.);
#3606=ORIENTED_EDGE('',*,*,#2645,.F.);
#3607=ORIENTED_EDGE('',*,*,#2648,.F.);
#3608=ORIENTED_EDGE('',*,*,#2423,.F.);
#3609=ORIENTED_EDGE('',*,*,#2419,.F.);
#3610=ORIENTED_EDGE('',*,*,#2751,.F.);
#3611=ORIENTED_EDGE('',*,*,#2428,.F.);
#3612=ORIENTED_EDGE('',*,*,#2432,.T.);
#3613=ORIENTED_EDGE('',*,*,#2650,.T.);
#3614=ORIENTED_EDGE('',*,*,#2653,.F.);
#3615=ORIENTED_EDGE('',*,*,#2656,.F.);
#3616=ORIENTED_EDGE('',*,*,#2437,.F.);
#3617=ORIENTED_EDGE('',*,*,#2433,.F.);
#3618=ORIENTED_EDGE('',*,*,#2752,.F.);
#3619=ORIENTED_EDGE('',*,*,#2442,.F.);
#3620=ORIENTED_EDGE('',*,*,#2446,.T.);
#3621=ORIENTED_EDGE('',*,*,#2658,.T.);
#3622=ORIENTED_EDGE('',*,*,#2661,.F.);
#3623=ORIENTED_EDGE('',*,*,#2664,.F.);
#3624=ORIENTED_EDGE('',*,*,#2451,.F.);
#3625=ORIENTED_EDGE('',*,*,#2447,.F.);
#3626=ORIENTED_EDGE('',*,*,#2753,.F.);
#3627=ORIENTED_EDGE('',*,*,#2456,.F.);
#3628=ORIENTED_EDGE('',*,*,#2460,.T.);
#3629=ORIENTED_EDGE('',*,*,#2666,.T.);
#3630=ORIENTED_EDGE('',*,*,#2669,.F.);
#3631=ORIENTED_EDGE('',*,*,#2672,.F.);
#3632=ORIENTED_EDGE('',*,*,#2465,.F.);
#3633=ORIENTED_EDGE('',*,*,#2461,.F.);
#3634=ORIENTED_EDGE('',*,*,#2754,.F.);
#3635=ORIENTED_EDGE('',*,*,#2470,.F.);
#3636=ORIENTED_EDGE('',*,*,#2474,.T.);
#3637=ORIENTED_EDGE('',*,*,#2674,.T.);
#3638=ORIENTED_EDGE('',*,*,#2677,.F.);
#3639=ORIENTED_EDGE('',*,*,#2680,.F.);
#3640=ORIENTED_EDGE('',*,*,#2479,.F.);
#3641=ORIENTED_EDGE('',*,*,#2475,.F.);
#3642=ORIENTED_EDGE('',*,*,#2755,.F.);
#3643=ORIENTED_EDGE('',*,*,#2484,.F.);
#3644=ORIENTED_EDGE('',*,*,#2488,.T.);
#3645=ORIENTED_EDGE('',*,*,#2682,.T.);
#3646=ORIENTED_EDGE('',*,*,#2685,.F.);
#3647=ORIENTED_EDGE('',*,*,#2688,.F.);
#3648=ORIENTED_EDGE('',*,*,#2493,.F.);
#3649=ORIENTED_EDGE('',*,*,#2489,.F.);
#3650=ORIENTED_EDGE('',*,*,#2756,.F.);
#3651=ORIENTED_EDGE('',*,*,#2498,.F.);
#3652=ORIENTED_EDGE('',*,*,#2502,.T.);
#3653=ORIENTED_EDGE('',*,*,#2690,.T.);
#3654=ORIENTED_EDGE('',*,*,#2693,.F.);
#3655=ORIENTED_EDGE('',*,*,#2696,.F.);
#3656=ORIENTED_EDGE('',*,*,#2507,.F.);
#3657=ORIENTED_EDGE('',*,*,#2503,.F.);
#3658=ORIENTED_EDGE('',*,*,#2757,.F.);
#3659=ORIENTED_EDGE('',*,*,#2512,.F.);
#3660=ORIENTED_EDGE('',*,*,#2516,.T.);
#3661=ORIENTED_EDGE('',*,*,#2698,.T.);
#3662=ORIENTED_EDGE('',*,*,#2701,.F.);
#3663=ORIENTED_EDGE('',*,*,#2704,.F.);
#3664=ORIENTED_EDGE('',*,*,#2521,.F.);
#3665=ORIENTED_EDGE('',*,*,#2517,.F.);
#3666=ORIENTED_EDGE('',*,*,#2758,.F.);
#3667=ORIENTED_EDGE('',*,*,#2526,.F.);
#3668=ORIENTED_EDGE('',*,*,#2530,.T.);
#3669=ORIENTED_EDGE('',*,*,#2706,.T.);
#3670=ORIENTED_EDGE('',*,*,#2709,.F.);
#3671=ORIENTED_EDGE('',*,*,#2712,.F.);
#3672=ORIENTED_EDGE('',*,*,#2535,.F.);
#3673=ORIENTED_EDGE('',*,*,#2531,.F.);
#3674=ORIENTED_EDGE('',*,*,#2759,.F.);
#3675=ORIENTED_EDGE('',*,*,#2540,.F.);
#3676=ORIENTED_EDGE('',*,*,#2544,.T.);
#3677=ORIENTED_EDGE('',*,*,#2714,.T.);
#3678=ORIENTED_EDGE('',*,*,#2717,.F.);
#3679=ORIENTED_EDGE('',*,*,#2720,.F.);
#3680=ORIENTED_EDGE('',*,*,#2549,.F.);
#3681=ORIENTED_EDGE('',*,*,#2545,.F.);
#3682=ORIENTED_EDGE('',*,*,#2760,.F.);
#3683=ORIENTED_EDGE('',*,*,#2554,.F.);
#3684=ORIENTED_EDGE('',*,*,#2558,.T.);
#3685=ORIENTED_EDGE('',*,*,#2722,.T.);
#3686=ORIENTED_EDGE('',*,*,#2725,.F.);
#3687=ORIENTED_EDGE('',*,*,#2728,.F.);
#3688=ORIENTED_EDGE('',*,*,#2563,.F.);
#3689=ORIENTED_EDGE('',*,*,#2559,.F.);
#3690=ORIENTED_EDGE('',*,*,#2761,.F.);
#3691=ORIENTED_EDGE('',*,*,#2568,.F.);
#3692=ORIENTED_EDGE('',*,*,#2572,.T.);
#3693=ORIENTED_EDGE('',*,*,#2730,.T.);
#3694=ORIENTED_EDGE('',*,*,#2733,.F.);
#3695=ORIENTED_EDGE('',*,*,#2736,.F.);
#3696=ORIENTED_EDGE('',*,*,#2577,.F.);
#3697=ORIENTED_EDGE('',*,*,#2573,.F.);
#3698=ORIENTED_EDGE('',*,*,#2762,.F.);
#3699=ORIENTED_EDGE('',*,*,#2582,.F.);
#3700=ORIENTED_EDGE('',*,*,#2586,.T.);
#3701=ORIENTED_EDGE('',*,*,#2738,.T.);
#3702=ORIENTED_EDGE('',*,*,#2741,.F.);
#3703=ORIENTED_EDGE('',*,*,#2744,.F.);
#3704=ORIENTED_EDGE('',*,*,#2591,.F.);
#3705=ORIENTED_EDGE('',*,*,#2587,.F.);
#3706=ORIENTED_EDGE('',*,*,#2763,.F.);
#3707=ORIENTED_EDGE('',*,*,#2764,.F.);
#3708=ORIENTED_EDGE('',*,*,#2765,.T.);
#3709=ORIENTED_EDGE('',*,*,#2766,.T.);
#3710=ORIENTED_EDGE('',*,*,#2767,.F.);
#3711=ORIENTED_EDGE('',*,*,#2768,.F.);
#3712=ORIENTED_EDGE('',*,*,#2769,.F.);
#3713=ORIENTED_EDGE('',*,*,#2770,.F.);
#3714=ORIENTED_EDGE('',*,*,#2771,.F.);
#3715=ORIENTED_EDGE('',*,*,#2330,.F.);
#3716=ORIENTED_EDGE('',*,*,#2334,.T.);
#3717=ORIENTED_EDGE('',*,*,#2594,.T.);
#3718=ORIENTED_EDGE('',*,*,#2597,.F.);
#3719=ORIENTED_EDGE('',*,*,#2600,.F.);
#3720=ORIENTED_EDGE('',*,*,#2339,.F.);
#3721=ORIENTED_EDGE('',*,*,#2335,.F.);
#3722=ORIENTED_EDGE('',*,*,#2772,.F.);
#3723=ORIENTED_EDGE('',*,*,#2327,.T.);
#3724=ORIENTED_EDGE('',*,*,#2773,.T.);
#3725=ORIENTED_EDGE('',*,*,#2774,.F.);
#3726=ORIENTED_EDGE('',*,*,#2775,.T.);
#3727=ORIENTED_EDGE('',*,*,#2776,.T.);
#3728=ORIENTED_EDGE('',*,*,#2777,.T.);
#3729=ORIENTED_EDGE('',*,*,#2778,.T.);
#3730=ORIENTED_EDGE('',*,*,#2779,.T.);
#3731=ORIENTED_EDGE('',*,*,#2780,.F.);
#3732=ORIENTED_EDGE('',*,*,#2781,.T.);
#3733=ORIENTED_EDGE('',*,*,#2589,.F.);
#3734=ORIENTED_EDGE('',*,*,#2593,.T.);
#3735=ORIENTED_EDGE('',*,*,#2745,.T.);
#3736=ORIENTED_EDGE('',*,*,#2742,.T.);
#3737=ORIENTED_EDGE('',*,*,#2739,.T.);
#3738=ORIENTED_EDGE('',*,*,#2584,.T.);
#3739=ORIENTED_EDGE('',*,*,#2580,.F.);
#3740=ORIENTED_EDGE('',*,*,#2782,.T.);
#3741=ORIENTED_EDGE('',*,*,#2575,.F.);
#3742=ORIENTED_EDGE('',*,*,#2579,.T.);
#3743=ORIENTED_EDGE('',*,*,#2737,.T.);
#3744=ORIENTED_EDGE('',*,*,#2734,.T.);
#3745=ORIENTED_EDGE('',*,*,#2731,.T.);
#3746=ORIENTED_EDGE('',*,*,#2570,.T.);
#3747=ORIENTED_EDGE('',*,*,#2566,.F.);
#3748=ORIENTED_EDGE('',*,*,#2783,.T.);
#3749=ORIENTED_EDGE('',*,*,#2561,.F.);
#3750=ORIENTED_EDGE('',*,*,#2565,.T.);
#3751=ORIENTED_EDGE('',*,*,#2729,.T.);
#3752=ORIENTED_EDGE('',*,*,#2726,.T.);
#3753=ORIENTED_EDGE('',*,*,#2723,.T.);
#3754=ORIENTED_EDGE('',*,*,#2556,.T.);
#3755=ORIENTED_EDGE('',*,*,#2552,.F.);
#3756=ORIENTED_EDGE('',*,*,#2784,.T.);
#3757=ORIENTED_EDGE('',*,*,#2547,.F.);
#3758=ORIENTED_EDGE('',*,*,#2551,.T.);
#3759=ORIENTED_EDGE('',*,*,#2721,.T.);
#3760=ORIENTED_EDGE('',*,*,#2718,.T.);
#3761=ORIENTED_EDGE('',*,*,#2715,.T.);
#3762=ORIENTED_EDGE('',*,*,#2542,.T.);
#3763=ORIENTED_EDGE('',*,*,#2538,.F.);
#3764=ORIENTED_EDGE('',*,*,#2785,.T.);
#3765=ORIENTED_EDGE('',*,*,#2533,.F.);
#3766=ORIENTED_EDGE('',*,*,#2537,.T.);
#3767=ORIENTED_EDGE('',*,*,#2713,.T.);
#3768=ORIENTED_EDGE('',*,*,#2710,.T.);
#3769=ORIENTED_EDGE('',*,*,#2707,.T.);
#3770=ORIENTED_EDGE('',*,*,#2528,.T.);
#3771=ORIENTED_EDGE('',*,*,#2524,.F.);
#3772=ORIENTED_EDGE('',*,*,#2786,.T.);
#3773=ORIENTED_EDGE('',*,*,#2519,.F.);
#3774=ORIENTED_EDGE('',*,*,#2523,.T.);
#3775=ORIENTED_EDGE('',*,*,#2705,.T.);
#3776=ORIENTED_EDGE('',*,*,#2702,.T.);
#3777=ORIENTED_EDGE('',*,*,#2699,.T.);
#3778=ORIENTED_EDGE('',*,*,#2514,.T.);
#3779=ORIENTED_EDGE('',*,*,#2510,.F.);
#3780=ORIENTED_EDGE('',*,*,#2787,.T.);
#3781=ORIENTED_EDGE('',*,*,#2505,.F.);
#3782=ORIENTED_EDGE('',*,*,#2509,.T.);
#3783=ORIENTED_EDGE('',*,*,#2697,.T.);
#3784=ORIENTED_EDGE('',*,*,#2694,.T.);
#3785=ORIENTED_EDGE('',*,*,#2691,.T.);
#3786=ORIENTED_EDGE('',*,*,#2500,.T.);
#3787=ORIENTED_EDGE('',*,*,#2496,.F.);
#3788=ORIENTED_EDGE('',*,*,#2788,.T.);
#3789=ORIENTED_EDGE('',*,*,#2491,.F.);
#3790=ORIENTED_EDGE('',*,*,#2495,.T.);
#3791=ORIENTED_EDGE('',*,*,#2689,.T.);
#3792=ORIENTED_EDGE('',*,*,#2686,.T.);
#3793=ORIENTED_EDGE('',*,*,#2683,.T.);
#3794=ORIENTED_EDGE('',*,*,#2486,.T.);
#3795=ORIENTED_EDGE('',*,*,#2482,.F.);
#3796=ORIENTED_EDGE('',*,*,#2789,.T.);
#3797=ORIENTED_EDGE('',*,*,#2477,.F.);
#3798=ORIENTED_EDGE('',*,*,#2481,.T.);
#3799=ORIENTED_EDGE('',*,*,#2681,.T.);
#3800=ORIENTED_EDGE('',*,*,#2678,.T.);
#3801=ORIENTED_EDGE('',*,*,#2675,.T.);
#3802=ORIENTED_EDGE('',*,*,#2472,.T.);
#3803=ORIENTED_EDGE('',*,*,#2468,.F.);
#3804=ORIENTED_EDGE('',*,*,#2790,.T.);
#3805=ORIENTED_EDGE('',*,*,#2463,.F.);
#3806=ORIENTED_EDGE('',*,*,#2467,.T.);
#3807=ORIENTED_EDGE('',*,*,#2673,.T.);
#3808=ORIENTED_EDGE('',*,*,#2670,.T.);
#3809=ORIENTED_EDGE('',*,*,#2667,.T.);
#3810=ORIENTED_EDGE('',*,*,#2458,.T.);
#3811=ORIENTED_EDGE('',*,*,#2454,.F.);
#3812=ORIENTED_EDGE('',*,*,#2791,.T.);
#3813=ORIENTED_EDGE('',*,*,#2449,.F.);
#3814=ORIENTED_EDGE('',*,*,#2453,.T.);
#3815=ORIENTED_EDGE('',*,*,#2665,.T.);
#3816=ORIENTED_EDGE('',*,*,#2662,.T.);
#3817=ORIENTED_EDGE('',*,*,#2659,.T.);
#3818=ORIENTED_EDGE('',*,*,#2444,.T.);
#3819=ORIENTED_EDGE('',*,*,#2440,.F.);
#3820=ORIENTED_EDGE('',*,*,#2792,.T.);
#3821=ORIENTED_EDGE('',*,*,#2435,.F.);
#3822=ORIENTED_EDGE('',*,*,#2439,.T.);
#3823=ORIENTED_EDGE('',*,*,#2657,.T.);
#3824=ORIENTED_EDGE('',*,*,#2654,.T.);
#3825=ORIENTED_EDGE('',*,*,#2651,.T.);
#3826=ORIENTED_EDGE('',*,*,#2430,.T.);
#3827=ORIENTED_EDGE('',*,*,#2426,.F.);
#3828=ORIENTED_EDGE('',*,*,#2793,.T.);
#3829=ORIENTED_EDGE('',*,*,#2421,.F.);
#3830=ORIENTED_EDGE('',*,*,#2425,.T.);
#3831=ORIENTED_EDGE('',*,*,#2649,.T.);
#3832=ORIENTED_EDGE('',*,*,#2646,.T.);
#3833=ORIENTED_EDGE('',*,*,#2643,.T.);
#3834=ORIENTED_EDGE('',*,*,#2416,.T.);
#3835=ORIENTED_EDGE('',*,*,#2412,.F.);
#3836=ORIENTED_EDGE('',*,*,#2794,.T.);
#3837=ORIENTED_EDGE('',*,*,#2407,.F.);
#3838=ORIENTED_EDGE('',*,*,#2411,.T.);
#3839=ORIENTED_EDGE('',*,*,#2641,.T.);
#3840=ORIENTED_EDGE('',*,*,#2638,.T.);
#3841=ORIENTED_EDGE('',*,*,#2635,.T.);
#3842=ORIENTED_EDGE('',*,*,#2402,.T.);
#3843=ORIENTED_EDGE('',*,*,#2398,.F.);
#3844=ORIENTED_EDGE('',*,*,#2795,.T.);
#3845=ORIENTED_EDGE('',*,*,#2393,.F.);
#3846=ORIENTED_EDGE('',*,*,#2397,.T.);
#3847=ORIENTED_EDGE('',*,*,#2633,.T.);
#3848=ORIENTED_EDGE('',*,*,#2630,.T.);
#3849=ORIENTED_EDGE('',*,*,#2627,.T.);
#3850=ORIENTED_EDGE('',*,*,#2388,.T.);
#3851=ORIENTED_EDGE('',*,*,#2384,.F.);
#3852=ORIENTED_EDGE('',*,*,#2796,.T.);
#3853=ORIENTED_EDGE('',*,*,#2379,.F.);
#3854=ORIENTED_EDGE('',*,*,#2383,.T.);
#3855=ORIENTED_EDGE('',*,*,#2625,.T.);
#3856=ORIENTED_EDGE('',*,*,#2622,.T.);
#3857=ORIENTED_EDGE('',*,*,#2619,.T.);
#3858=ORIENTED_EDGE('',*,*,#2374,.T.);
#3859=ORIENTED_EDGE('',*,*,#2370,.F.);
#3860=ORIENTED_EDGE('',*,*,#2797,.T.);
#3861=ORIENTED_EDGE('',*,*,#2365,.F.);
#3862=ORIENTED_EDGE('',*,*,#2369,.T.);
#3863=ORIENTED_EDGE('',*,*,#2617,.T.);
#3864=ORIENTED_EDGE('',*,*,#2614,.T.);
#3865=ORIENTED_EDGE('',*,*,#2611,.T.);
#3866=ORIENTED_EDGE('',*,*,#2360,.T.);
#3867=ORIENTED_EDGE('',*,*,#2356,.F.);
#3868=ORIENTED_EDGE('',*,*,#2798,.T.);
#3869=ORIENTED_EDGE('',*,*,#2351,.F.);
#3870=ORIENTED_EDGE('',*,*,#2355,.T.);
#3871=ORIENTED_EDGE('',*,*,#2609,.T.);
#3872=ORIENTED_EDGE('',*,*,#2606,.T.);
#3873=ORIENTED_EDGE('',*,*,#2603,.T.);
#3874=ORIENTED_EDGE('',*,*,#2346,.T.);
#3875=ORIENTED_EDGE('',*,*,#2342,.F.);
#3876=ORIENTED_EDGE('',*,*,#2799,.T.);
#3877=ORIENTED_EDGE('',*,*,#2337,.F.);
#3878=ORIENTED_EDGE('',*,*,#2341,.T.);
#3879=ORIENTED_EDGE('',*,*,#2601,.T.);
#3880=ORIENTED_EDGE('',*,*,#2598,.T.);
#3881=ORIENTED_EDGE('',*,*,#2595,.T.);
#3882=ORIENTED_EDGE('',*,*,#2332,.T.);
#3883=ORIENTED_EDGE('',*,*,#2328,.F.);
#3884=ORIENTED_EDGE('',*,*,#2325,.T.);
#3885=ORIENTED_EDGE('',*,*,#2590,.F.);
#3886=ORIENTED_EDGE('',*,*,#2781,.F.);
#3887=ORIENTED_EDGE('',*,*,#2800,.F.);
#3888=ORIENTED_EDGE('',*,*,#2763,.T.);
#3889=ORIENTED_EDGE('',*,*,#2576,.F.);
#3890=ORIENTED_EDGE('',*,*,#2782,.F.);
#3891=ORIENTED_EDGE('',*,*,#2583,.F.);
#3892=ORIENTED_EDGE('',*,*,#2762,.T.);
#3893=ORIENTED_EDGE('',*,*,#2562,.F.);
#3894=ORIENTED_EDGE('',*,*,#2783,.F.);
#3895=ORIENTED_EDGE('',*,*,#2569,.F.);
#3896=ORIENTED_EDGE('',*,*,#2761,.T.);
#3897=ORIENTED_EDGE('',*,*,#2548,.F.);
#3898=ORIENTED_EDGE('',*,*,#2784,.F.);
#3899=ORIENTED_EDGE('',*,*,#2555,.F.);
#3900=ORIENTED_EDGE('',*,*,#2760,.T.);
#3901=ORIENTED_EDGE('',*,*,#2534,.F.);
#3902=ORIENTED_EDGE('',*,*,#2785,.F.);
#3903=ORIENTED_EDGE('',*,*,#2541,.F.);
#3904=ORIENTED_EDGE('',*,*,#2759,.T.);
#3905=ORIENTED_EDGE('',*,*,#2520,.F.);
#3906=ORIENTED_EDGE('',*,*,#2786,.F.);
#3907=ORIENTED_EDGE('',*,*,#2527,.F.);
#3908=ORIENTED_EDGE('',*,*,#2758,.T.);
#3909=ORIENTED_EDGE('',*,*,#2506,.F.);
#3910=ORIENTED_EDGE('',*,*,#2787,.F.);
#3911=ORIENTED_EDGE('',*,*,#2513,.F.);
#3912=ORIENTED_EDGE('',*,*,#2757,.T.);
#3913=ORIENTED_EDGE('',*,*,#2492,.F.);
#3914=ORIENTED_EDGE('',*,*,#2788,.F.);
#3915=ORIENTED_EDGE('',*,*,#2499,.F.);
#3916=ORIENTED_EDGE('',*,*,#2756,.T.);
#3917=ORIENTED_EDGE('',*,*,#2478,.F.);
#3918=ORIENTED_EDGE('',*,*,#2789,.F.);
#3919=ORIENTED_EDGE('',*,*,#2485,.F.);
#3920=ORIENTED_EDGE('',*,*,#2755,.T.);
#3921=ORIENTED_EDGE('',*,*,#2464,.F.);
#3922=ORIENTED_EDGE('',*,*,#2790,.F.);
#3923=ORIENTED_EDGE('',*,*,#2471,.F.);
#3924=ORIENTED_EDGE('',*,*,#2754,.T.);
#3925=ORIENTED_EDGE('',*,*,#2450,.F.);
#3926=ORIENTED_EDGE('',*,*,#2791,.F.);
#3927=ORIENTED_EDGE('',*,*,#2457,.F.);
#3928=ORIENTED_EDGE('',*,*,#2753,.T.);
#3929=ORIENTED_EDGE('',*,*,#2436,.F.);
#3930=ORIENTED_EDGE('',*,*,#2792,.F.);
#3931=ORIENTED_EDGE('',*,*,#2443,.F.);
#3932=ORIENTED_EDGE('',*,*,#2752,.T.);
#3933=ORIENTED_EDGE('',*,*,#2422,.F.);
#3934=ORIENTED_EDGE('',*,*,#2793,.F.);
#3935=ORIENTED_EDGE('',*,*,#2429,.F.);
#3936=ORIENTED_EDGE('',*,*,#2751,.T.);
#3937=ORIENTED_EDGE('',*,*,#2408,.F.);
#3938=ORIENTED_EDGE('',*,*,#2794,.F.);
#3939=ORIENTED_EDGE('',*,*,#2415,.F.);
#3940=ORIENTED_EDGE('',*,*,#2750,.T.);
#3941=ORIENTED_EDGE('',*,*,#2394,.F.);
#3942=ORIENTED_EDGE('',*,*,#2795,.F.);
#3943=ORIENTED_EDGE('',*,*,#2401,.F.);
#3944=ORIENTED_EDGE('',*,*,#2749,.T.);
#3945=ORIENTED_EDGE('',*,*,#2380,.F.);
#3946=ORIENTED_EDGE('',*,*,#2796,.F.);
#3947=ORIENTED_EDGE('',*,*,#2387,.F.);
#3948=ORIENTED_EDGE('',*,*,#2748,.T.);
#3949=ORIENTED_EDGE('',*,*,#2366,.F.);
#3950=ORIENTED_EDGE('',*,*,#2797,.F.);
#3951=ORIENTED_EDGE('',*,*,#2373,.F.);
#3952=ORIENTED_EDGE('',*,*,#2747,.T.);
#3953=ORIENTED_EDGE('',*,*,#2352,.F.);
#3954=ORIENTED_EDGE('',*,*,#2798,.F.);
#3955=ORIENTED_EDGE('',*,*,#2359,.F.);
#3956=ORIENTED_EDGE('',*,*,#2746,.T.);
#3957=ORIENTED_EDGE('',*,*,#2338,.F.);
#3958=ORIENTED_EDGE('',*,*,#2799,.F.);
#3959=ORIENTED_EDGE('',*,*,#2345,.F.);
#3960=ORIENTED_EDGE('',*,*,#2772,.T.);
#3961=ORIENTED_EDGE('',*,*,#2780,.T.);
#3962=ORIENTED_EDGE('',*,*,#2801,.T.);
#3963=ORIENTED_EDGE('',*,*,#2764,.T.);
#3964=ORIENTED_EDGE('',*,*,#2800,.T.);
#3965=ORIENTED_EDGE('',*,*,#2801,.F.);
#3966=ORIENTED_EDGE('',*,*,#2779,.F.);
#3967=ORIENTED_EDGE('',*,*,#2802,.F.);
#3968=ORIENTED_EDGE('',*,*,#2765,.F.);
#3969=ORIENTED_EDGE('',*,*,#2770,.T.);
#3970=ORIENTED_EDGE('',*,*,#2803,.T.);
#3971=ORIENTED_EDGE('',*,*,#2774,.T.);
#3972=ORIENTED_EDGE('',*,*,#2804,.T.);
#3973=ORIENTED_EDGE('',*,*,#2803,.F.);
#3974=ORIENTED_EDGE('',*,*,#2769,.T.);
#3975=ORIENTED_EDGE('',*,*,#2805,.T.);
#3976=ORIENTED_EDGE('',*,*,#2775,.F.);
#3977=ORIENTED_EDGE('',*,*,#2766,.F.);
#3978=ORIENTED_EDGE('',*,*,#2802,.T.);
#3979=ORIENTED_EDGE('',*,*,#2778,.F.);
#3980=ORIENTED_EDGE('',*,*,#2806,.F.);
#3981=ORIENTED_EDGE('',*,*,#2767,.T.);
#3982=ORIENTED_EDGE('',*,*,#2806,.T.);
#3983=ORIENTED_EDGE('',*,*,#2777,.F.);
#3984=ORIENTED_EDGE('',*,*,#2807,.F.);
#3985=ORIENTED_EDGE('',*,*,#2768,.T.);
#3986=ORIENTED_EDGE('',*,*,#2807,.T.);
#3987=ORIENTED_EDGE('',*,*,#2776,.F.);
#3988=ORIENTED_EDGE('',*,*,#2805,.F.);
#3989=ORIENTED_EDGE('',*,*,#2331,.F.);
#3990=ORIENTED_EDGE('',*,*,#2771,.T.);
#3991=ORIENTED_EDGE('',*,*,#2804,.F.);
#3992=ORIENTED_EDGE('',*,*,#2773,.F.);
#3993=ORIENTED_EDGE('',*,*,#2808,.F.);
#3994=ORIENTED_EDGE('',*,*,#2809,.T.);
#3995=ORIENTED_EDGE('',*,*,#2810,.F.);
#3996=ORIENTED_EDGE('',*,*,#2809,.F.);
#3997=ORIENTED_EDGE('',*,*,#2811,.T.);
#3998=ORIENTED_EDGE('',*,*,#2812,.T.);
#3999=ORIENTED_EDGE('',*,*,#2813,.T.);
#4000=ORIENTED_EDGE('',*,*,#2812,.F.);
#4001=ORIENTED_EDGE('',*,*,#2814,.T.);
#4002=ORIENTED_EDGE('',*,*,#2815,.T.);
#4003=ORIENTED_EDGE('',*,*,#2813,.F.);
#4004=ORIENTED_EDGE('',*,*,#2815,.F.);
#4005=ORIENTED_EDGE('',*,*,#2808,.T.);
#4006=ORIENTED_EDGE('',*,*,#2816,.T.);
#4007=ORIENTED_EDGE('',*,*,#2811,.F.);
#4008=ORIENTED_EDGE('',*,*,#2816,.F.);
#4009=ORIENTED_EDGE('',*,*,#2817,.F.);
#4010=ORIENTED_EDGE('',*,*,#2818,.F.);
#4011=ORIENTED_EDGE('',*,*,#2819,.T.);
#4012=ORIENTED_EDGE('',*,*,#2819,.F.);
#4013=ORIENTED_EDGE('',*,*,#2820,.F.);
#4014=ORIENTED_EDGE('',*,*,#2821,.T.);
#4015=ORIENTED_EDGE('',*,*,#2821,.F.);
#4016=ORIENTED_EDGE('',*,*,#2822,.F.);
#4017=ORIENTED_EDGE('',*,*,#2823,.T.);
#4018=ORIENTED_EDGE('',*,*,#2823,.F.);
#4019=ORIENTED_EDGE('',*,*,#2824,.F.);
#4020=ORIENTED_EDGE('',*,*,#2825,.T.);
#4021=ORIENTED_EDGE('',*,*,#2825,.F.);
#4022=ORIENTED_EDGE('',*,*,#2826,.F.);
#4023=ORIENTED_EDGE('',*,*,#2827,.T.);
#4024=ORIENTED_EDGE('',*,*,#2827,.F.);
#4025=ORIENTED_EDGE('',*,*,#2828,.F.);
#4026=ORIENTED_EDGE('',*,*,#2817,.T.);
#4027=ORIENTED_EDGE('',*,*,#2829,.F.);
#4028=ORIENTED_EDGE('',*,*,#2830,.T.);
#4029=ORIENTED_EDGE('',*,*,#2818,.T.);
#4030=ORIENTED_EDGE('',*,*,#2831,.F.);
#4031=ORIENTED_EDGE('',*,*,#2832,.F.);
#4032=ORIENTED_EDGE('',*,*,#2833,.T.);
#4033=ORIENTED_EDGE('',*,*,#2820,.T.);
#4034=ORIENTED_EDGE('',*,*,#2830,.F.);
#4035=ORIENTED_EDGE('',*,*,#2834,.F.);
#4036=ORIENTED_EDGE('',*,*,#2835,.T.);
#4037=ORIENTED_EDGE('',*,*,#2822,.T.);
#4038=ORIENTED_EDGE('',*,*,#2833,.F.);
#4039=ORIENTED_EDGE('',*,*,#2836,.F.);
#4040=ORIENTED_EDGE('',*,*,#2837,.T.);
#4041=ORIENTED_EDGE('',*,*,#2824,.T.);
#4042=ORIENTED_EDGE('',*,*,#2835,.F.);
#4043=ORIENTED_EDGE('',*,*,#2838,.F.);
#4044=ORIENTED_EDGE('',*,*,#2839,.T.);
#4045=ORIENTED_EDGE('',*,*,#2826,.T.);
#4046=ORIENTED_EDGE('',*,*,#2837,.F.);
#4047=ORIENTED_EDGE('',*,*,#2840,.F.);
#4048=ORIENTED_EDGE('',*,*,#2831,.T.);
#4049=ORIENTED_EDGE('',*,*,#2828,.T.);
#4050=ORIENTED_EDGE('',*,*,#2839,.F.);
#4051=ORIENTED_EDGE('',*,*,#2841,.F.);
#4052=ORIENTED_EDGE('',*,*,#2829,.T.);
#4053=ORIENTED_EDGE('',*,*,#2840,.T.);
#4054=ORIENTED_EDGE('',*,*,#2838,.T.);
#4055=ORIENTED_EDGE('',*,*,#2836,.T.);
#4056=ORIENTED_EDGE('',*,*,#2834,.T.);
#4057=ORIENTED_EDGE('',*,*,#2832,.T.);
#4058=ORIENTED_EDGE('',*,*,#2814,.F.);
#4059=ORIENTED_EDGE('',*,*,#2842,.T.);
#4060=ORIENTED_EDGE('',*,*,#2841,.T.);
#4061=ORIENTED_EDGE('',*,*,#2842,.F.);
#4062=ORIENTED_EDGE('',*,*,#2810,.T.);
#4063=ORIENTED_EDGE('',*,*,#2843,.F.);
#4064=ORIENTED_EDGE('',*,*,#2844,.T.);
#4065=ORIENTED_EDGE('',*,*,#2845,.F.);
#4066=ORIENTED_EDGE('',*,*,#2844,.F.);
#4067=ORIENTED_EDGE('',*,*,#2846,.T.);
#4068=ORIENTED_EDGE('',*,*,#2847,.T.);
#4069=ORIENTED_EDGE('',*,*,#2848,.T.);
#4070=ORIENTED_EDGE('',*,*,#2847,.F.);
#4071=ORIENTED_EDGE('',*,*,#2849,.T.);
#4072=ORIENTED_EDGE('',*,*,#2850,.T.);
#4073=ORIENTED_EDGE('',*,*,#2848,.F.);
#4074=ORIENTED_EDGE('',*,*,#2850,.F.);
#4075=ORIENTED_EDGE('',*,*,#2843,.T.);
#4076=ORIENTED_EDGE('',*,*,#2851,.T.);
#4077=ORIENTED_EDGE('',*,*,#2846,.F.);
#4078=ORIENTED_EDGE('',*,*,#2851,.F.);
#4079=ORIENTED_EDGE('',*,*,#2852,.F.);
#4080=ORIENTED_EDGE('',*,*,#2853,.F.);
#4081=ORIENTED_EDGE('',*,*,#2854,.T.);
#4082=ORIENTED_EDGE('',*,*,#2854,.F.);
#4083=ORIENTED_EDGE('',*,*,#2855,.F.);
#4084=ORIENTED_EDGE('',*,*,#2856,.T.);
#4085=ORIENTED_EDGE('',*,*,#2856,.F.);
#4086=ORIENTED_EDGE('',*,*,#2857,.F.);
#4087=ORIENTED_EDGE('',*,*,#2858,.T.);
#4088=ORIENTED_EDGE('',*,*,#2858,.F.);
#4089=ORIENTED_EDGE('',*,*,#2859,.F.);
#4090=ORIENTED_EDGE('',*,*,#2860,.T.);
#4091=ORIENTED_EDGE('',*,*,#2860,.F.);
#4092=ORIENTED_EDGE('',*,*,#2861,.F.);
#4093=ORIENTED_EDGE('',*,*,#2862,.T.);
#4094=ORIENTED_EDGE('',*,*,#2862,.F.);
#4095=ORIENTED_EDGE('',*,*,#2863,.F.);
#4096=ORIENTED_EDGE('',*,*,#2852,.T.);
#4097=ORIENTED_EDGE('',*,*,#2864,.F.);
#4098=ORIENTED_EDGE('',*,*,#2865,.T.);
#4099=ORIENTED_EDGE('',*,*,#2853,.T.);
#4100=ORIENTED_EDGE('',*,*,#2866,.F.);
#4101=ORIENTED_EDGE('',*,*,#2867,.F.);
#4102=ORIENTED_EDGE('',*,*,#2868,.T.);
#4103=ORIENTED_EDGE('',*,*,#2855,.T.);
#4104=ORIENTED_EDGE('',*,*,#2865,.F.);
#4105=ORIENTED_EDGE('',*,*,#2869,.F.);
#4106=ORIENTED_EDGE('',*,*,#2870,.T.);
#4107=ORIENTED_EDGE('',*,*,#2857,.T.);
#4108=ORIENTED_EDGE('',*,*,#2868,.F.);
#4109=ORIENTED_EDGE('',*,*,#2871,.F.);
#4110=ORIENTED_EDGE('',*,*,#2872,.T.);
#4111=ORIENTED_EDGE('',*,*,#2859,.T.);
#4112=ORIENTED_EDGE('',*,*,#2870,.F.);
#4113=ORIENTED_EDGE('',*,*,#2873,.F.);
#4114=ORIENTED_EDGE('',*,*,#2874,.T.);
#4115=ORIENTED_EDGE('',*,*,#2861,.T.);
#4116=ORIENTED_EDGE('',*,*,#2872,.F.);
#4117=ORIENTED_EDGE('',*,*,#2875,.F.);
#4118=ORIENTED_EDGE('',*,*,#2866,.T.);
#4119=ORIENTED_EDGE('',*,*,#2863,.T.);
#4120=ORIENTED_EDGE('',*,*,#2874,.F.);
#4121=ORIENTED_EDGE('',*,*,#2876,.F.);
#4122=ORIENTED_EDGE('',*,*,#2864,.T.);
#4123=ORIENTED_EDGE('',*,*,#2875,.T.);
#4124=ORIENTED_EDGE('',*,*,#2873,.T.);
#4125=ORIENTED_EDGE('',*,*,#2871,.T.);
#4126=ORIENTED_EDGE('',*,*,#2869,.T.);
#4127=ORIENTED_EDGE('',*,*,#2867,.T.);
#4128=ORIENTED_EDGE('',*,*,#2849,.F.);
#4129=ORIENTED_EDGE('',*,*,#2877,.T.);
#4130=ORIENTED_EDGE('',*,*,#2876,.T.);
#4131=ORIENTED_EDGE('',*,*,#2877,.F.);
#4132=ORIENTED_EDGE('',*,*,#2845,.T.);
#4133=ORIENTED_EDGE('',*,*,#2878,.T.);
#4134=ORIENTED_EDGE('',*,*,#2879,.T.);
#4135=ORIENTED_EDGE('',*,*,#2880,.F.);
#4136=ORIENTED_EDGE('',*,*,#2879,.F.);
#4137=ORIENTED_EDGE('',*,*,#2881,.T.);
#4138=ORIENTED_EDGE('',*,*,#2878,.F.);
#4139=ORIENTED_EDGE('',*,*,#2882,.F.);
#4140=ORIENTED_EDGE('',*,*,#2883,.T.);
#4141=ORIENTED_EDGE('',*,*,#2884,.T.);
#4142=ORIENTED_EDGE('',*,*,#2883,.F.);
#4143=ORIENTED_EDGE('',*,*,#2881,.F.);
#4144=ORIENTED_EDGE('',*,*,#2885,.T.);
#4145=ORIENTED_EDGE('',*,*,#2882,.T.);
#4146=ORIENTED_EDGE('',*,*,#2885,.F.);
#4147=ORIENTED_EDGE('',*,*,#2886,.F.);
#4148=ORIENTED_EDGE('',*,*,#2887,.F.);
#4149=ORIENTED_EDGE('',*,*,#2888,.T.);
#4150=ORIENTED_EDGE('',*,*,#2886,.T.);
#4151=ORIENTED_EDGE('',*,*,#2888,.F.);
#4152=ORIENTED_EDGE('',*,*,#2887,.T.);
#4153=ORIENTED_EDGE('',*,*,#2884,.F.);
#4154=ORIENTED_EDGE('',*,*,#2880,.T.);
#4155=ORIENTED_EDGE('',*,*,#2889,.T.);
#4156=ORIENTED_EDGE('',*,*,#2890,.T.);
#4157=ORIENTED_EDGE('',*,*,#2891,.T.);
#4158=ORIENTED_EDGE('',*,*,#2890,.F.);
#4159=ORIENTED_EDGE('',*,*,#2891,.F.);
#4160=ORIENTED_EDGE('',*,*,#2892,.T.);
#4161=ORIENTED_EDGE('',*,*,#2893,.T.);
#4162=ORIENTED_EDGE('',*,*,#2892,.F.);
#4163=ORIENTED_EDGE('',*,*,#2889,.F.);
#4164=ORIENTED_EDGE('',*,*,#2894,.F.);
#4165=ORIENTED_EDGE('',*,*,#2895,.T.);
#4166=ORIENTED_EDGE('',*,*,#2896,.T.);
#4167=ORIENTED_EDGE('',*,*,#2897,.T.);
#4168=ORIENTED_EDGE('',*,*,#2896,.F.);
#4169=ORIENTED_EDGE('',*,*,#2898,.F.);
#4170=ORIENTED_EDGE('',*,*,#2897,.F.);
#4171=ORIENTED_EDGE('',*,*,#2899,.F.);
#4172=ORIENTED_EDGE('',*,*,#2900,.T.);
#4173=ORIENTED_EDGE('',*,*,#2895,.F.);
#4174=ORIENTED_EDGE('',*,*,#2900,.F.);
#4175=ORIENTED_EDGE('',*,*,#2898,.T.);
#4176=ORIENTED_EDGE('',*,*,#2901,.T.);
#4177=ORIENTED_EDGE('',*,*,#2902,.T.);
#4178=ORIENTED_EDGE('',*,*,#2901,.F.);
#4179=ORIENTED_EDGE('',*,*,#2902,.F.);
#4180=ORIENTED_EDGE('',*,*,#2903,.T.);
#4181=ORIENTED_EDGE('',*,*,#2904,.T.);
#4182=ORIENTED_EDGE('',*,*,#2903,.F.);
#4183=ORIENTED_EDGE('',*,*,#2899,.T.);
#4184=ORIENTED_EDGE('',*,*,#2893,.F.);
#4185=ORIENTED_EDGE('',*,*,#2905,.F.);
#4186=ORIENTED_EDGE('',*,*,#2906,.T.);
#4187=ORIENTED_EDGE('',*,*,#2894,.T.);
#4188=ORIENTED_EDGE('',*,*,#2906,.F.);
#4189=ORIENTED_EDGE('',*,*,#2907,.F.);
#4190=ORIENTED_EDGE('',*,*,#2908,.T.);
#4191=ORIENTED_EDGE('',*,*,#2905,.T.);
#4192=ORIENTED_EDGE('',*,*,#2908,.F.);
#4193=ORIENTED_EDGE('',*,*,#2909,.F.);
#4194=ORIENTED_EDGE('',*,*,#2907,.T.);
#4195=ORIENTED_EDGE('',*,*,#2910,.F.);
#4196=ORIENTED_EDGE('',*,*,#2911,.T.);
#4197=ORIENTED_EDGE('',*,*,#2909,.T.);
#4198=ORIENTED_EDGE('',*,*,#2911,.F.);
#4199=ORIENTED_EDGE('',*,*,#2912,.F.);
#4200=ORIENTED_EDGE('',*,*,#2910,.T.);
#4201=ORIENTED_EDGE('',*,*,#2913,.F.);
#4202=ORIENTED_EDGE('',*,*,#2914,.T.);
#4203=ORIENTED_EDGE('',*,*,#2912,.T.);
#4204=ORIENTED_EDGE('',*,*,#2914,.F.);
#4205=ORIENTED_EDGE('',*,*,#2915,.F.);
#4206=ORIENTED_EDGE('',*,*,#2913,.T.);
#4207=ORIENTED_EDGE('',*,*,#2916,.F.);
#4208=ORIENTED_EDGE('',*,*,#2917,.T.);
#4209=ORIENTED_EDGE('',*,*,#2915,.T.);
#4210=ORIENTED_EDGE('',*,*,#2917,.F.);
#4211=ORIENTED_EDGE('',*,*,#2904,.F.);
#4212=ORIENTED_EDGE('',*,*,#2916,.T.);
#4213=ORIENTED_EDGE('',*,*,#2918,.F.);
#4214=ORIENTED_EDGE('',*,*,#2919,.F.);
#4215=ORIENTED_EDGE('',*,*,#2920,.F.);
#4216=ORIENTED_EDGE('',*,*,#2921,.F.);
#4217=ORIENTED_EDGE('',*,*,#2922,.F.);
#4218=ORIENTED_EDGE('',*,*,#2923,.F.);
#4219=ORIENTED_EDGE('',*,*,#2924,.F.);
#4220=ORIENTED_EDGE('',*,*,#2925,.F.);
#4221=ORIENTED_EDGE('',*,*,#2924,.T.);
#4222=ORIENTED_EDGE('',*,*,#2918,.T.);
#4223=ORIENTED_EDGE('',*,*,#2926,.F.);
#4224=ORIENTED_EDGE('',*,*,#2927,.F.);
#4225=ORIENTED_EDGE('',*,*,#2928,.F.);
#4226=ORIENTED_EDGE('',*,*,#2929,.F.);
#4227=ORIENTED_EDGE('',*,*,#2930,.F.);
#4228=ORIENTED_EDGE('',*,*,#2927,.T.);
#4229=ORIENTED_EDGE('',*,*,#2922,.T.);
#4230=ORIENTED_EDGE('',*,*,#2931,.F.);
#4231=ORIENTED_EDGE('',*,*,#2932,.F.);
#4232=ORIENTED_EDGE('',*,*,#2933,.F.);
#4233=ORIENTED_EDGE('',*,*,#2934,.T.);
#4234=ORIENTED_EDGE('',*,*,#2935,.T.);
#4235=ORIENTED_EDGE('',*,*,#2936,.T.);
#4236=ORIENTED_EDGE('',*,*,#2921,.T.);
#4237=ORIENTED_EDGE('',*,*,#2926,.T.);
#4238=ORIENTED_EDGE('',*,*,#2936,.F.);
#4239=ORIENTED_EDGE('',*,*,#2937,.F.);
#4240=ORIENTED_EDGE('',*,*,#2938,.F.);
#4241=ORIENTED_EDGE('',*,*,#2925,.T.);
#4242=ORIENTED_EDGE('',*,*,#2938,.T.);
#4243=ORIENTED_EDGE('',*,*,#2939,.T.);
#4244=ORIENTED_EDGE('',*,*,#2940,.T.);
#4245=ORIENTED_EDGE('',*,*,#2941,.T.);
#4246=ORIENTED_EDGE('',*,*,#2942,.T.);
#4247=ORIENTED_EDGE('',*,*,#2943,.T.);
#4248=ORIENTED_EDGE('',*,*,#2931,.T.);
#4249=ORIENTED_EDGE('',*,*,#2942,.F.);
#4250=ORIENTED_EDGE('',*,*,#2944,.T.);
#4251=ORIENTED_EDGE('',*,*,#2945,.F.);
#4252=ORIENTED_EDGE('',*,*,#2928,.T.);
#4253=ORIENTED_EDGE('',*,*,#2945,.T.);
#4254=ORIENTED_EDGE('',*,*,#2946,.T.);
#4255=ORIENTED_EDGE('',*,*,#2947,.T.);
#4256=ORIENTED_EDGE('',*,*,#2948,.F.);
#4257=ORIENTED_EDGE('',*,*,#2949,.F.);
#4258=ORIENTED_EDGE('',*,*,#2950,.F.);
#4259=ORIENTED_EDGE('',*,*,#2939,.F.);
#4260=ORIENTED_EDGE('',*,*,#2937,.T.);
#4261=ORIENTED_EDGE('',*,*,#2951,.F.);
#4262=ORIENTED_EDGE('',*,*,#2952,.F.);
#4263=ORIENTED_EDGE('',*,*,#2940,.F.);
#4264=ORIENTED_EDGE('',*,*,#2950,.T.);
#4265=ORIENTED_EDGE('',*,*,#2953,.F.);
#4266=ORIENTED_EDGE('',*,*,#2944,.F.);
#4267=ORIENTED_EDGE('',*,*,#2941,.F.);
#4268=ORIENTED_EDGE('',*,*,#2952,.T.);
#4269=ORIENTED_EDGE('',*,*,#2954,.F.);
#4270=ORIENTED_EDGE('',*,*,#2955,.F.);
#4271=ORIENTED_EDGE('',*,*,#2956,.T.);
#4272=ORIENTED_EDGE('',*,*,#2943,.F.);
#4273=ORIENTED_EDGE('',*,*,#2956,.F.);
#4274=ORIENTED_EDGE('',*,*,#2957,.T.);
#4275=ORIENTED_EDGE('',*,*,#2958,.T.);
#4276=ORIENTED_EDGE('',*,*,#2955,.T.);
#4277=ORIENTED_EDGE('',*,*,#2958,.F.);
#4278=ORIENTED_EDGE('',*,*,#2951,.T.);
#4279=ORIENTED_EDGE('',*,*,#2935,.F.);
#4280=ORIENTED_EDGE('',*,*,#2959,.F.);
#4281=ORIENTED_EDGE('',*,*,#2960,.F.);
#4282=ORIENTED_EDGE('',*,*,#2953,.T.);
#4283=ORIENTED_EDGE('',*,*,#2960,.T.);
#4284=ORIENTED_EDGE('',*,*,#2961,.T.);
#4285=ORIENTED_EDGE('',*,*,#2962,.T.);
#4286=ORIENTED_EDGE('',*,*,#2954,.T.);
#4287=ORIENTED_EDGE('',*,*,#2962,.F.);
#4288=ORIENTED_EDGE('',*,*,#2963,.F.);
#4289=ORIENTED_EDGE('',*,*,#2946,.F.);
#4290=ORIENTED_EDGE('',*,*,#2919,.T.);
#4291=ORIENTED_EDGE('',*,*,#2923,.T.);
#4292=ORIENTED_EDGE('',*,*,#2930,.T.);
#4293=ORIENTED_EDGE('',*,*,#2964,.F.);
#4294=ORIENTED_EDGE('',*,*,#2948,.T.);
#4295=ORIENTED_EDGE('',*,*,#2965,.T.);
#4296=ORIENTED_EDGE('',*,*,#2966,.T.);
#4297=ORIENTED_EDGE('',*,*,#2967,.F.);
#4298=ORIENTED_EDGE('',*,*,#2933,.T.);
#4299=ORIENTED_EDGE('',*,*,#2968,.F.);
#4300=ORIENTED_EDGE('',*,*,#2969,.T.);
#4301=ORIENTED_EDGE('',*,*,#2970,.T.);
#4302=ORIENTED_EDGE('',*,*,#2971,.T.);
#4303=ORIENTED_EDGE('',*,*,#2972,.T.);
#4304=ORIENTED_EDGE('',*,*,#2973,.T.);
#4305=ORIENTED_EDGE('',*,*,#2974,.T.);
#4306=ORIENTED_EDGE('',*,*,#2975,.T.);
#4307=ORIENTED_EDGE('',*,*,#2976,.T.);
#4308=ORIENTED_EDGE('',*,*,#2977,.T.);
#4309=ORIENTED_EDGE('',*,*,#2978,.T.);
#4310=ORIENTED_EDGE('',*,*,#2977,.F.);
#4311=ORIENTED_EDGE('',*,*,#2979,.T.);
#4312=ORIENTED_EDGE('',*,*,#2971,.F.);
#4313=ORIENTED_EDGE('',*,*,#2980,.T.);
#4314=ORIENTED_EDGE('',*,*,#2981,.T.);
#4315=ORIENTED_EDGE('',*,*,#2982,.T.);
#4316=ORIENTED_EDGE('',*,*,#2983,.T.);
#4317=ORIENTED_EDGE('',*,*,#2980,.F.);
#4318=ORIENTED_EDGE('',*,*,#2984,.T.);
#4319=ORIENTED_EDGE('',*,*,#2975,.F.);
#4320=ORIENTED_EDGE('',*,*,#2985,.T.);
#4321=ORIENTED_EDGE('',*,*,#2972,.F.);
#4322=ORIENTED_EDGE('',*,*,#2986,.F.);
#4323=ORIENTED_EDGE('',*,*,#2987,.F.);
#4324=ORIENTED_EDGE('',*,*,#2988,.F.);
#4325=ORIENTED_EDGE('',*,*,#2969,.F.);
#4326=ORIENTED_EDGE('',*,*,#2979,.F.);
#4327=ORIENTED_EDGE('',*,*,#2989,.T.);
#4328=ORIENTED_EDGE('',*,*,#2990,.T.);
#4329=ORIENTED_EDGE('',*,*,#2986,.T.);
#4330=ORIENTED_EDGE('',*,*,#2976,.F.);
#4331=ORIENTED_EDGE('',*,*,#2991,.F.);
#4332=ORIENTED_EDGE('',*,*,#2992,.F.);
#4333=ORIENTED_EDGE('',*,*,#2993,.F.);
#4334=ORIENTED_EDGE('',*,*,#2994,.F.);
#4335=ORIENTED_EDGE('',*,*,#2989,.F.);
#4336=ORIENTED_EDGE('',*,*,#2995,.F.);
#4337=ORIENTED_EDGE('',*,*,#2984,.F.);
#4338=ORIENTED_EDGE('',*,*,#2996,.T.);
#4339=ORIENTED_EDGE('',*,*,#2997,.F.);
#4340=ORIENTED_EDGE('',*,*,#2991,.T.);
#4341=ORIENTED_EDGE('',*,*,#2983,.F.);
#4342=ORIENTED_EDGE('',*,*,#2998,.T.);
#4343=ORIENTED_EDGE('',*,*,#2966,.F.);
#4344=ORIENTED_EDGE('',*,*,#2999,.F.);
#4345=ORIENTED_EDGE('',*,*,#3000,.F.);
#4346=ORIENTED_EDGE('',*,*,#2996,.F.);
#4347=ORIENTED_EDGE('',*,*,#3001,.T.);
#4348=ORIENTED_EDGE('',*,*,#3002,.T.);
#4349=ORIENTED_EDGE('',*,*,#2990,.F.);
#4350=ORIENTED_EDGE('',*,*,#2994,.T.);
#4351=ORIENTED_EDGE('',*,*,#3003,.T.);
#4352=ORIENTED_EDGE('',*,*,#3004,.T.);
#4353=ORIENTED_EDGE('',*,*,#3001,.F.);
#4354=ORIENTED_EDGE('',*,*,#2993,.T.);
#4355=ORIENTED_EDGE('',*,*,#2997,.T.);
#4356=ORIENTED_EDGE('',*,*,#3005,.T.);
#4357=ORIENTED_EDGE('',*,*,#3003,.F.);
#4358=ORIENTED_EDGE('',*,*,#2992,.T.);
#4359=ORIENTED_EDGE('',*,*,#3006,.T.);
#4360=ORIENTED_EDGE('',*,*,#3007,.T.);
#4361=ORIENTED_EDGE('',*,*,#2995,.T.);
#4362=ORIENTED_EDGE('',*,*,#3007,.F.);
#4363=ORIENTED_EDGE('',*,*,#3006,.F.);
#4364=ORIENTED_EDGE('',*,*,#3008,.T.);
#4365=ORIENTED_EDGE('',*,*,#3009,.F.);
#4366=ORIENTED_EDGE('',*,*,#3008,.F.);
#4367=ORIENTED_EDGE('',*,*,#3002,.F.);
#4368=ORIENTED_EDGE('',*,*,#3010,.T.);
#4369=ORIENTED_EDGE('',*,*,#3011,.T.);
#4370=ORIENTED_EDGE('',*,*,#2987,.T.);
#4371=ORIENTED_EDGE('',*,*,#3004,.F.);
#4372=ORIENTED_EDGE('',*,*,#3012,.F.);
#4373=ORIENTED_EDGE('',*,*,#3013,.F.);
#4374=ORIENTED_EDGE('',*,*,#3010,.F.);
#4375=ORIENTED_EDGE('',*,*,#3005,.F.);
#4376=ORIENTED_EDGE('',*,*,#3000,.T.);
#4377=ORIENTED_EDGE('',*,*,#3014,.T.);
#4378=ORIENTED_EDGE('',*,*,#3012,.T.);
#4379=ORIENTED_EDGE('',*,*,#2974,.F.);
#4380=ORIENTED_EDGE('',*,*,#3015,.T.);
#4381=ORIENTED_EDGE('',*,*,#2981,.F.);
#4382=ORIENTED_EDGE('',*,*,#2978,.F.);
#4383=ORIENTED_EDGE('',*,*,#3016,.F.);
#4384=ORIENTED_EDGE('',*,*,#3017,.T.);
#4385=ORIENTED_EDGE('',*,*,#3018,.T.);
#4386=ORIENTED_EDGE('',*,*,#3017,.F.);
#4387=ORIENTED_EDGE('',*,*,#3016,.T.);
#4388=ORIENTED_EDGE('',*,*,#2988,.T.);
#4389=ORIENTED_EDGE('',*,*,#3011,.F.);
#4390=ORIENTED_EDGE('',*,*,#3013,.T.);
#4391=ORIENTED_EDGE('',*,*,#3014,.F.);
#4392=ORIENTED_EDGE('',*,*,#2999,.T.);
#4393=ORIENTED_EDGE('',*,*,#2965,.F.);
#4394=ORIENTED_EDGE('',*,*,#2947,.F.);
#4395=ORIENTED_EDGE('',*,*,#2963,.T.);
#4396=ORIENTED_EDGE('',*,*,#2961,.F.);
#4397=ORIENTED_EDGE('',*,*,#2959,.T.);
#4398=ORIENTED_EDGE('',*,*,#2934,.F.);
#4399=ORIENTED_EDGE('',*,*,#2970,.F.);
#4400=ORIENTED_EDGE('',*,*,#2957,.F.);
#4401=ORIENTED_EDGE('',*,*,#3009,.T.);
#4402=ORIENTED_EDGE('',*,*,#2968,.T.);
#4403=ORIENTED_EDGE('',*,*,#2932,.T.);
#4404=ORIENTED_EDGE('',*,*,#2920,.T.);
#4405=ORIENTED_EDGE('',*,*,#2964,.T.);
#4406=ORIENTED_EDGE('',*,*,#2929,.T.);
#4407=ORIENTED_EDGE('',*,*,#2949,.T.);
#4408=ORIENTED_EDGE('',*,*,#2967,.T.);
#4409=ORIENTED_EDGE('',*,*,#2998,.F.);
#4410=ORIENTED_EDGE('',*,*,#2982,.F.);
#4411=ORIENTED_EDGE('',*,*,#3015,.F.);
#4412=ORIENTED_EDGE('',*,*,#2973,.F.);
#4413=ORIENTED_EDGE('',*,*,#2985,.F.);
#4414=ORIENTED_EDGE('',*,*,#3019,.F.);
#4415=ORIENTED_EDGE('',*,*,#3020,.F.);
#4416=ORIENTED_EDGE('',*,*,#3021,.T.);
#4417=ORIENTED_EDGE('',*,*,#3019,.T.);
#4418=ORIENTED_EDGE('',*,*,#3021,.F.);
#4419=ORIENTED_EDGE('',*,*,#3020,.T.);
#4420=ORIENTED_EDGE('',*,*,#3022,.F.);
#4421=ORIENTED_EDGE('',*,*,#3023,.F.);
#4422=ORIENTED_EDGE('',*,*,#3024,.T.);
#4423=ORIENTED_EDGE('',*,*,#3022,.T.);
#4424=ORIENTED_EDGE('',*,*,#3024,.F.);
#4425=ORIENTED_EDGE('',*,*,#3023,.T.);
#4426=ORIENTED_EDGE('',*,*,#3018,.F.);
#4427=ORIENTED_EDGE('',*,*,#3025,.F.);
#4428=ORIENTED_EDGE('',*,*,#3026,.T.);
#4429=ORIENTED_EDGE('',*,*,#3025,.T.);
#4430=ORIENTED_EDGE('',*,*,#3026,.F.);
#4431=CYLINDRICAL_SURFACE('',#4912,5.);
#4432=CYLINDRICAL_SURFACE('',#4915,1.);
#4433=CYLINDRICAL_SURFACE('',#4919,1.);
#4434=CYLINDRICAL_SURFACE('',#4923,1.);
#4435=CYLINDRICAL_SURFACE('',#4927,1.);
#4436=CYLINDRICAL_SURFACE('',#4931,1.);
#4437=CYLINDRICAL_SURFACE('',#4935,1.);
#4438=CYLINDRICAL_SURFACE('',#4939,1.);
#4439=CYLINDRICAL_SURFACE('',#4943,1.);
#4440=CYLINDRICAL_SURFACE('',#4947,1.);
#4441=CYLINDRICAL_SURFACE('',#4951,1.);
#4442=CYLINDRICAL_SURFACE('',#4955,1.);
#4443=CYLINDRICAL_SURFACE('',#4959,1.);
#4444=CYLINDRICAL_SURFACE('',#4963,1.);
#4445=CYLINDRICAL_SURFACE('',#4967,1.);
#4446=CYLINDRICAL_SURFACE('',#4971,1.);
#4447=CYLINDRICAL_SURFACE('',#4975,1.);
#4448=CYLINDRICAL_SURFACE('',#4979,1.);
#4449=CYLINDRICAL_SURFACE('',#4983,1.);
#4450=CYLINDRICAL_SURFACE('',#4987,1.);
#4451=CYLINDRICAL_SURFACE('',#4991,1.);
#4452=CYLINDRICAL_SURFACE('',#4995,1.);
#4453=CYLINDRICAL_SURFACE('',#4999,1.);
#4454=CYLINDRICAL_SURFACE('',#5003,1.);
#4455=CYLINDRICAL_SURFACE('',#5007,1.);
#4456=CYLINDRICAL_SURFACE('',#5011,1.);
#4457=CYLINDRICAL_SURFACE('',#5015,1.);
#4458=CYLINDRICAL_SURFACE('',#5019,1.);
#4459=CYLINDRICAL_SURFACE('',#5023,1.);
#4460=CYLINDRICAL_SURFACE('',#5027,1.);
#4461=CYLINDRICAL_SURFACE('',#5031,1.);
#4462=CYLINDRICAL_SURFACE('',#5035,1.);
#4463=CYLINDRICAL_SURFACE('',#5039,1.);
#4464=CYLINDRICAL_SURFACE('',#5043,1.);
#4465=CYLINDRICAL_SURFACE('',#5047,1.);
#4466=CYLINDRICAL_SURFACE('',#5051,1.);
#4467=CYLINDRICAL_SURFACE('',#5055,1.);
#4468=CYLINDRICAL_SURFACE('',#5059,1.);
#4469=CYLINDRICAL_SURFACE('',#5063,1.);
#4470=CYLINDRICAL_SURFACE('',#5067,21.9999999999943);
#4471=CYLINDRICAL_SURFACE('',#5070,21.9999999999943);
#4472=CYLINDRICAL_SURFACE('',#5073,21.9999999999943);
#4473=CYLINDRICAL_SURFACE('',#5076,21.9999999999943);
#4474=CYLINDRICAL_SURFACE('',#5079,21.9999999999943);
#4475=CYLINDRICAL_SURFACE('',#5082,21.9999999999943);
#4476=CYLINDRICAL_SURFACE('',#5085,21.9999999999943);
#4477=CYLINDRICAL_SURFACE('',#5088,21.9999999999943);
#4478=CYLINDRICAL_SURFACE('',#5091,21.9999999999943);
#4479=CYLINDRICAL_SURFACE('',#5094,21.9999999999943);
#4480=CYLINDRICAL_SURFACE('',#5097,21.9999999999943);
#4481=CYLINDRICAL_SURFACE('',#5100,21.9999999999943);
#4482=CYLINDRICAL_SURFACE('',#5103,21.9999999999943);
#4483=CYLINDRICAL_SURFACE('',#5106,21.9999999999943);
#4484=CYLINDRICAL_SURFACE('',#5109,21.9999999999943);
#4485=CYLINDRICAL_SURFACE('',#5112,21.9999999999943);
#4486=CYLINDRICAL_SURFACE('',#5115,21.9999999999943);
#4487=CYLINDRICAL_SURFACE('',#5118,21.9999999999943);
#4488=CYLINDRICAL_SURFACE('',#5121,21.9999999999943);
#4489=CYLINDRICAL_SURFACE('',#5172,17.686);
#4490=CYLINDRICAL_SURFACE('',#5173,17.686);
#4491=CYLINDRICAL_SURFACE('',#5174,17.686);
#4492=CYLINDRICAL_SURFACE('',#5175,17.686);
#4493=CYLINDRICAL_SURFACE('',#5176,17.686);
#4494=CYLINDRICAL_SURFACE('',#5177,17.686);
#4495=CYLINDRICAL_SURFACE('',#5178,17.686);
#4496=CYLINDRICAL_SURFACE('',#5179,17.686);
#4497=CYLINDRICAL_SURFACE('',#5180,17.686);
#4498=CYLINDRICAL_SURFACE('',#5181,17.686);
#4499=CYLINDRICAL_SURFACE('',#5182,17.686);
#4500=CYLINDRICAL_SURFACE('',#5183,17.686);
#4501=CYLINDRICAL_SURFACE('',#5184,17.686);
#4502=CYLINDRICAL_SURFACE('',#5185,17.686);
#4503=CYLINDRICAL_SURFACE('',#5186,17.686);
#4504=CYLINDRICAL_SURFACE('',#5187,17.686);
#4505=CYLINDRICAL_SURFACE('',#5188,17.686);
#4506=CYLINDRICAL_SURFACE('',#5189,17.686);
#4507=CYLINDRICAL_SURFACE('',#5190,17.686);
#4508=CYLINDRICAL_SURFACE('',#5191,1.);
#4509=CYLINDRICAL_SURFACE('',#5193,1.);
#4510=CYLINDRICAL_SURFACE('',#5195,21.9999999999943);
#4511=CYLINDRICAL_SURFACE('',#5196,17.686);
#4512=CYLINDRICAL_SURFACE('',#5207,7.911);
#4513=CYLINDRICAL_SURFACE('',#5222,14.48);
#4514=CYLINDRICAL_SURFACE('',#5234,7.911);
#4515=CYLINDRICAL_SURFACE('',#5249,14.48);
#4516=CYLINDRICAL_SURFACE('',#5252,5.);
#4517=CYLINDRICAL_SURFACE('',#5261,11.);
#4518=CYLINDRICAL_SURFACE('',#5264,27.4027293621977);
#4519=CYLINDRICAL_SURFACE('',#5273,19.7498324643894);
#4520=CYLINDRICAL_SURFACE('',#5283,26.6934256722844);
#4521=CYLINDRICAL_SURFACE('',#5288,33.);
#4522=CYLINDRICAL_SURFACE('',#5291,11.);
#4523=CYLINDRICAL_SURFACE('',#5298,27.4027293621977);
#4524=CYLINDRICAL_SURFACE('',#5302,29.0578798664922);
#4525=CYLINDRICAL_SURFACE('',#5306,31.1192710879259);
#4526=CYLINDRICAL_SURFACE('',#5310,1.);
#4527=CYLINDRICAL_SURFACE('',#5320,1.);
#4528=CYLINDRICAL_SURFACE('',#5326,1.);
#4529=CYLINDRICAL_SURFACE('',#5332,1.);
#4530=CYLINDRICAL_SURFACE('',#5338,1.);
#4531=CYLINDRICAL_SURFACE('',#5344,8.8273485245745);
#4532=CYLINDRICAL_SURFACE('',#5346,5.);
#4533=CYLINDRICAL_SURFACE('',#5349,5.);
#4534=CYLINDRICAL_SURFACE('',#5351,38.889325151227);
#4535=CYLINDRICAL_SURFACE('',#5353,33.);
#4536=CYLINDRICAL_SURFACE('',#5356,33.);
#4537=CYLINDRICAL_SURFACE('',#5359,1.);
#4538=CYLINDRICAL_SURFACE('',#5369,1.);
#4539=CYLINDRICAL_SURFACE('',#5375,1.);
#4540=CYLINDRICAL_SURFACE('',#5381,1.);
#4541=CYLINDRICAL_SURFACE('',#5387,1.);
#4542=CYLINDRICAL_SURFACE('',#5393,8.8273485245745);
#4543=CYLINDRICAL_SURFACE('',#5395,5.);
#4544=CYLINDRICAL_SURFACE('',#5398,5.);
#4545=CYLINDRICAL_SURFACE('',#5400,38.889325151227);
#4546=CYLINDRICAL_SURFACE('',#5402,27.4027293621977);
#4547=CYLINDRICAL_SURFACE('',#5409,31.1192710879259);
#4548=CYLINDRICAL_SURFACE('',#5413,29.0578798664922);
#4549=ADVANCED_FACE('',(#325),#4431,.F.);
#4550=ADVANCED_FACE('',(#326),#4432,.F.);
#4551=ADVANCED_FACE('',(#327),#231,.T.);
#4552=ADVANCED_FACE('',(#328),#4433,.F.);
#4553=ADVANCED_FACE('',(#329),#232,.T.);
#4554=ADVANCED_FACE('',(#330),#4434,.F.);
#4555=ADVANCED_FACE('',(#331),#233,.T.);
#4556=ADVANCED_FACE('',(#332),#4435,.F.);
#4557=ADVANCED_FACE('',(#333),#234,.T.);
#4558=ADVANCED_FACE('',(#334),#4436,.F.);
#4559=ADVANCED_FACE('',(#335),#235,.T.);
#4560=ADVANCED_FACE('',(#336),#4437,.F.);
#4561=ADVANCED_FACE('',(#337),#236,.T.);
#4562=ADVANCED_FACE('',(#338),#4438,.F.);
#4563=ADVANCED_FACE('',(#339),#237,.T.);
#4564=ADVANCED_FACE('',(#340),#4439,.F.);
#4565=ADVANCED_FACE('',(#341),#238,.T.);
#4566=ADVANCED_FACE('',(#342),#4440,.F.);
#4567=ADVANCED_FACE('',(#343),#239,.T.);
#4568=ADVANCED_FACE('',(#344),#4441,.F.);
#4569=ADVANCED_FACE('',(#345),#240,.T.);
#4570=ADVANCED_FACE('',(#346),#4442,.F.);
#4571=ADVANCED_FACE('',(#347),#241,.T.);
#4572=ADVANCED_FACE('',(#348),#4443,.F.);
#4573=ADVANCED_FACE('',(#349),#242,.T.);
#4574=ADVANCED_FACE('',(#350),#4444,.F.);
#4575=ADVANCED_FACE('',(#351),#243,.T.);
#4576=ADVANCED_FACE('',(#352),#4445,.F.);
#4577=ADVANCED_FACE('',(#353),#244,.T.);
#4578=ADVANCED_FACE('',(#354),#4446,.F.);
#4579=ADVANCED_FACE('',(#355),#245,.T.);
#4580=ADVANCED_FACE('',(#356),#4447,.F.);
#4581=ADVANCED_FACE('',(#357),#246,.T.);
#4582=ADVANCED_FACE('',(#358),#4448,.F.);
#4583=ADVANCED_FACE('',(#359),#247,.T.);
#4584=ADVANCED_FACE('',(#360),#4449,.F.);
#4585=ADVANCED_FACE('',(#361),#248,.T.);
#4586=ADVANCED_FACE('',(#362),#4450,.F.);
#4587=ADVANCED_FACE('',(#363),#249,.T.);
#4588=ADVANCED_FACE('',(#364),#4451,.F.);
#4589=ADVANCED_FACE('',(#365),#250,.T.);
#4590=ADVANCED_FACE('',(#366),#4452,.F.);
#4591=ADVANCED_FACE('',(#367),#251,.T.);
#4592=ADVANCED_FACE('',(#368),#4453,.F.);
#4593=ADVANCED_FACE('',(#369),#252,.T.);
#4594=ADVANCED_FACE('',(#370),#4454,.F.);
#4595=ADVANCED_FACE('',(#371),#253,.T.);
#4596=ADVANCED_FACE('',(#372),#4455,.F.);
#4597=ADVANCED_FACE('',(#373),#254,.T.);
#4598=ADVANCED_FACE('',(#374),#4456,.F.);
#4599=ADVANCED_FACE('',(#375),#255,.T.);
#4600=ADVANCED_FACE('',(#376),#4457,.F.);
#4601=ADVANCED_FACE('',(#377),#256,.T.);
#4602=ADVANCED_FACE('',(#378),#4458,.F.);
#4603=ADVANCED_FACE('',(#379),#257,.T.);
#4604=ADVANCED_FACE('',(#380),#4459,.F.);
#4605=ADVANCED_FACE('',(#381),#258,.T.);
#4606=ADVANCED_FACE('',(#382),#4460,.F.);
#4607=ADVANCED_FACE('',(#383),#259,.T.);
#4608=ADVANCED_FACE('',(#384),#4461,.F.);
#4609=ADVANCED_FACE('',(#385),#260,.T.);
#4610=ADVANCED_FACE('',(#386),#4462,.F.);
#4611=ADVANCED_FACE('',(#387),#261,.T.);
#4612=ADVANCED_FACE('',(#388),#4463,.F.);
#4613=ADVANCED_FACE('',(#389),#262,.T.);
#4614=ADVANCED_FACE('',(#390),#4464,.F.);
#4615=ADVANCED_FACE('',(#391),#263,.T.);
#4616=ADVANCED_FACE('',(#392),#4465,.F.);
#4617=ADVANCED_FACE('',(#393),#264,.T.);
#4618=ADVANCED_FACE('',(#394),#4466,.F.);
#4619=ADVANCED_FACE('',(#395),#265,.T.);
#4620=ADVANCED_FACE('',(#396),#4467,.F.);
#4621=ADVANCED_FACE('',(#397),#266,.T.);
#4622=ADVANCED_FACE('',(#398),#4468,.F.);
#4623=ADVANCED_FACE('',(#399),#267,.T.);
#4624=ADVANCED_FACE('',(#400),#4469,.F.);
#4625=ADVANCED_FACE('',(#401),#268,.T.);
#4626=ADVANCED_FACE('',(#402),#191,.T.);
#4627=ADVANCED_FACE('',(#403),#4470,.T.);
#4628=ADVANCED_FACE('',(#404),#192,.T.);
#4629=ADVANCED_FACE('',(#405),#193,.T.);
#4630=ADVANCED_FACE('',(#406),#4471,.T.);
#4631=ADVANCED_FACE('',(#407),#194,.T.);
#4632=ADVANCED_FACE('',(#408),#195,.T.);
#4633=ADVANCED_FACE('',(#409),#4472,.T.);
#4634=ADVANCED_FACE('',(#410),#196,.T.);
#4635=ADVANCED_FACE('',(#411),#197,.T.);
#4636=ADVANCED_FACE('',(#412),#4473,.T.);
#4637=ADVANCED_FACE('',(#413),#198,.T.);
#4638=ADVANCED_FACE('',(#414),#199,.T.);
#4639=ADVANCED_FACE('',(#415),#4474,.T.);
#4640=ADVANCED_FACE('',(#416),#200,.T.);
#4641=ADVANCED_FACE('',(#417),#201,.T.);
#4642=ADVANCED_FACE('',(#418),#4475,.T.);
#4643=ADVANCED_FACE('',(#419),#202,.T.);
#4644=ADVANCED_FACE('',(#420),#203,.T.);
#4645=ADVANCED_FACE('',(#421),#4476,.T.);
#4646=ADVANCED_FACE('',(#422),#204,.T.);
#4647=ADVANCED_FACE('',(#423),#205,.T.);
#4648=ADVANCED_FACE('',(#424),#4477,.T.);
#4649=ADVANCED_FACE('',(#425),#206,.T.);
#4650=ADVANCED_FACE('',(#426),#207,.T.);
#4651=ADVANCED_FACE('',(#427),#4478,.T.);
#4652=ADVANCED_FACE('',(#428),#208,.T.);
#4653=ADVANCED_FACE('',(#429),#209,.T.);
#4654=ADVANCED_FACE('',(#430),#4479,.T.);
#4655=ADVANCED_FACE('',(#431),#210,.T.);
#4656=ADVANCED_FACE('',(#432),#211,.T.);
#4657=ADVANCED_FACE('',(#433),#4480,.T.);
#4658=ADVANCED_FACE('',(#434),#212,.T.);
#4659=ADVANCED_FACE('',(#435),#213,.T.);
#4660=ADVANCED_FACE('',(#436),#4481,.T.);
#4661=ADVANCED_FACE('',(#437),#214,.T.);
#4662=ADVANCED_FACE('',(#438),#215,.T.);
#4663=ADVANCED_FACE('',(#439),#4482,.T.);
#4664=ADVANCED_FACE('',(#440),#216,.T.);
#4665=ADVANCED_FACE('',(#441),#217,.T.);
#4666=ADVANCED_FACE('',(#442),#4483,.T.);
#4667=ADVANCED_FACE('',(#443),#218,.T.);
#4668=ADVANCED_FACE('',(#444),#219,.T.);
#4669=ADVANCED_FACE('',(#445),#4484,.T.);
#4670=ADVANCED_FACE('',(#446),#220,.T.);
#4671=ADVANCED_FACE('',(#447),#221,.T.);
#4672=ADVANCED_FACE('',(#448),#4485,.T.);
#4673=ADVANCED_FACE('',(#449),#222,.T.);
#4674=ADVANCED_FACE('',(#450),#223,.T.);
#4675=ADVANCED_FACE('',(#451),#4486,.T.);
#4676=ADVANCED_FACE('',(#452),#224,.T.);
#4677=ADVANCED_FACE('',(#453),#225,.T.);
#4678=ADVANCED_FACE('',(#454),#4487,.T.);
#4679=ADVANCED_FACE('',(#455),#226,.T.);
#4680=ADVANCED_FACE('',(#456),#227,.T.);
#4681=ADVANCED_FACE('',(#457),#4488,.T.);
#4682=ADVANCED_FACE('',(#458),#228,.T.);
#4683=ADVANCED_FACE('',(#459,#91),#269,.F.);
#4684=ADVANCED_FACE('',(#460,#92),#270,.T.);
#4685=ADVANCED_FACE('',(#461),#4489,.T.);
#4686=ADVANCED_FACE('',(#462),#4490,.T.);
#4687=ADVANCED_FACE('',(#463),#4491,.T.);
#4688=ADVANCED_FACE('',(#464),#4492,.T.);
#4689=ADVANCED_FACE('',(#465),#4493,.T.);
#4690=ADVANCED_FACE('',(#466),#4494,.T.);
#4691=ADVANCED_FACE('',(#467),#4495,.T.);
#4692=ADVANCED_FACE('',(#468),#4496,.T.);
#4693=ADVANCED_FACE('',(#469),#4497,.T.);
#4694=ADVANCED_FACE('',(#470),#4498,.T.);
#4695=ADVANCED_FACE('',(#471),#4499,.T.);
#4696=ADVANCED_FACE('',(#472),#4500,.T.);
#4697=ADVANCED_FACE('',(#473),#4501,.T.);
#4698=ADVANCED_FACE('',(#474),#4502,.T.);
#4699=ADVANCED_FACE('',(#475),#4503,.T.);
#4700=ADVANCED_FACE('',(#476),#4504,.T.);
#4701=ADVANCED_FACE('',(#477),#4505,.T.);
#4702=ADVANCED_FACE('',(#478),#4506,.T.);
#4703=ADVANCED_FACE('',(#479),#4507,.T.);
#4704=ADVANCED_FACE('',(#480),#4508,.F.);
#4705=ADVANCED_FACE('',(#481),#271,.T.);
#4706=ADVANCED_FACE('',(#482),#4509,.F.);
#4707=ADVANCED_FACE('',(#483),#272,.T.);
#4708=ADVANCED_FACE('',(#484),#229,.T.);
#4709=ADVANCED_FACE('',(#485),#4510,.T.);
#4710=ADVANCED_FACE('',(#486),#230,.T.);
#4711=ADVANCED_FACE('',(#487),#4511,.T.);
#4712=ADVANCED_FACE('',(#488),#57,.T.);
#4713=ADVANCED_FACE('',(#489),#43,.F.);
#4714=ADVANCED_FACE('',(#490),#58,.T.);
#4715=ADVANCED_FACE('',(#491),#4512,.T.);
#4716=ADVANCED_FACE('',(#492),#273,.F.);
#4717=ADVANCED_FACE('',(#493),#274,.F.);
#4718=ADVANCED_FACE('',(#494),#275,.F.);
#4719=ADVANCED_FACE('',(#495),#276,.F.);
#4720=ADVANCED_FACE('',(#496),#277,.F.);
#4721=ADVANCED_FACE('',(#497),#278,.F.);
#4722=ADVANCED_FACE('',(#498),#279,.F.);
#4723=ADVANCED_FACE('',(#499),#280,.F.);
#4724=ADVANCED_FACE('',(#500),#281,.F.);
#4725=ADVANCED_FACE('',(#501),#282,.F.);
#4726=ADVANCED_FACE('',(#502),#283,.F.);
#4727=ADVANCED_FACE('',(#503),#284,.F.);
#4728=ADVANCED_FACE('',(#504,#93),#285,.T.);
#4729=ADVANCED_FACE('',(#505),#4513,.T.);
#4730=ADVANCED_FACE('',(#506),#286,.T.);
#4731=ADVANCED_FACE('',(#507),#59,.T.);
#4732=ADVANCED_FACE('',(#508),#44,.F.);
#4733=ADVANCED_FACE('',(#509),#60,.T.);
#4734=ADVANCED_FACE('',(#510),#4514,.T.);
#4735=ADVANCED_FACE('',(#511),#287,.F.);
#4736=ADVANCED_FACE('',(#512),#288,.F.);
#4737=ADVANCED_FACE('',(#513),#289,.F.);
#4738=ADVANCED_FACE('',(#514),#290,.F.);
#4739=ADVANCED_FACE('',(#515),#291,.F.);
#4740=ADVANCED_FACE('',(#516),#292,.F.);
#4741=ADVANCED_FACE('',(#517),#293,.F.);
#4742=ADVANCED_FACE('',(#518),#294,.F.);
#4743=ADVANCED_FACE('',(#519),#295,.F.);
#4744=ADVANCED_FACE('',(#520),#296,.F.);
#4745=ADVANCED_FACE('',(#521),#297,.F.);
#4746=ADVANCED_FACE('',(#522),#298,.F.);
#4747=ADVANCED_FACE('',(#523,#94),#299,.T.);
#4748=ADVANCED_FACE('',(#524),#4515,.T.);
#4749=ADVANCED_FACE('',(#525),#300,.T.);
#4750=ADVANCED_FACE('',(#526),#4516,.T.);
#4751=ADVANCED_FACE('',(#527,#95),#301,.T.);
#4752=ADVANCED_FACE('',(#528),#45,.F.);
#4753=ADVANCED_FACE('',(#529),#4517,.T.);
#4754=ADVANCED_FACE('',(#530),#302,.T.);
#4755=ADVANCED_FACE('',(#531),#4518,.T.);
#4756=ADVANCED_FACE('',(#532,#96),#303,.T.);
#4757=ADVANCED_FACE('',(#533),#304,.T.);
#4758=ADVANCED_FACE('',(#534),#46,.T.);
#4759=ADVANCED_FACE('',(#535),#4519,.T.);
#4760=ADVANCED_FACE('',(#536,#97),#305,.T.);
#4761=ADVANCED_FACE('',(#537),#47,.T.);
#4762=ADVANCED_FACE('',(#538,#98),#306,.T.);
#4763=ADVANCED_FACE('',(#539),#4520,.F.);
#4764=ADVANCED_FACE('',(#540),#48,.T.);
#4765=ADVANCED_FACE('',(#541),#4521,.T.);
#4766=ADVANCED_FACE('',(#542,#99),#307,.T.);
#4767=ADVANCED_FACE('',(#543),#4522,.F.);
#4768=ADVANCED_FACE('',(#544),#49,.F.);
#4769=ADVANCED_FACE('',(#545,#100),#308,.T.);
#4770=ADVANCED_FACE('',(#546),#4523,.T.);
#4771=ADVANCED_FACE('',(#547,#101),#309,.T.);
#4772=ADVANCED_FACE('',(#548),#4524,.F.);
#4773=ADVANCED_FACE('',(#549,#102),#310,.T.);
#4774=ADVANCED_FACE('',(#550),#4525,.F.);
#4775=ADVANCED_FACE('',(#551,#103),#311,.T.);
#4776=ADVANCED_FACE('',(#552),#4526,.T.);
#4777=ADVANCED_FACE('',(#553),#50,.T.);
#4778=ADVANCED_FACE('',(#554),#39,.T.);
#4779=ADVANCED_FACE('',(#555),#4527,.T.);
#4780=ADVANCED_FACE('',(#556),#40,.T.);
#4781=ADVANCED_FACE('',(#557),#312,.F.);
#4782=ADVANCED_FACE('',(#558),#4528,.T.);
#4783=ADVANCED_FACE('',(#559,#104),#313,.F.);
#4784=ADVANCED_FACE('',(#560),#4529,.T.);
#4785=ADVANCED_FACE('',(#561),#314,.F.);
#4786=ADVANCED_FACE('',(#562),#51,.T.);
#4787=ADVANCED_FACE('',(#563),#4530,.T.);
#4788=ADVANCED_FACE('',(#564),#52,.T.);
#4789=ADVANCED_FACE('',(#565),#61,.F.);
#4790=ADVANCED_FACE('',(#566),#4531,.F.);
#4791=ADVANCED_FACE('',(#567),#4532,.T.);
#4792=ADVANCED_FACE('',(#568),#315,.F.);
#4793=ADVANCED_FACE('',(#569),#4533,.T.);
#4794=ADVANCED_FACE('',(#570),#4534,.F.);
#4795=ADVANCED_FACE('',(#571),#4535,.T.);
#4796=ADVANCED_FACE('',(#572),#4536,.T.);
#4797=ADVANCED_FACE('',(#573),#4537,.T.);
#4798=ADVANCED_FACE('',(#574),#53,.T.);
#4799=ADVANCED_FACE('',(#575),#41,.T.);
#4800=ADVANCED_FACE('',(#576),#4538,.T.);
#4801=ADVANCED_FACE('',(#577),#42,.T.);
#4802=ADVANCED_FACE('',(#578),#316,.T.);
#4803=ADVANCED_FACE('',(#579),#4539,.T.);
#4804=ADVANCED_FACE('',(#580,#105),#317,.T.);
#4805=ADVANCED_FACE('',(#581),#4540,.T.);
#4806=ADVANCED_FACE('',(#582),#318,.T.);
#4807=ADVANCED_FACE('',(#583),#54,.T.);
#4808=ADVANCED_FACE('',(#584),#4541,.T.);
#4809=ADVANCED_FACE('',(#585),#55,.T.);
#4810=ADVANCED_FACE('',(#586),#62,.F.);
#4811=ADVANCED_FACE('',(#587),#4542,.F.);
#4812=ADVANCED_FACE('',(#588),#4543,.T.);
#4813=ADVANCED_FACE('',(#589),#319,.T.);
#4814=ADVANCED_FACE('',(#590),#4544,.T.);
#4815=ADVANCED_FACE('',(#591),#4545,.F.);
#4816=ADVANCED_FACE('',(#592),#4546,.F.);
#4817=ADVANCED_FACE('',(#593),#320,.T.);
#4818=ADVANCED_FACE('',(#594,#106,#107),#321,.T.);
#4819=ADVANCED_FACE('',(#595,#108),#322,.T.);
#4820=ADVANCED_FACE('',(#596),#4547,.T.);
#4821=ADVANCED_FACE('',(#597,#109),#323,.T.);
#4822=ADVANCED_FACE('',(#598),#4548,.T.);
#4823=ADVANCED_FACE('',(#599,#110),#324,.T.);
#4824=ADVANCED_FACE('',(#600),#56,.T.);
#4825=CLOSED_SHELL('',(#4549,#4550,#4551,#4552,#4553,#4554,#4555,#4556,
#4557,#4558,#4559,#4560,#4561,#4562,#4563,#4564,#4565,#4566,#4567,#4568,
#4569,#4570,#4571,#4572,#4573,#4574,#4575,#4576,#4577,#4578,#4579,#4580,
#4581,#4582,#4583,#4584,#4585,#4586,#4587,#4588,#4589,#4590,#4591,#4592,
#4593,#4594,#4595,#4596,#4597,#4598,#4599,#4600,#4601,#4602,#4603,#4604,
#4605,#4606,#4607,#4608,#4609,#4610,#4611,#4612,#4613,#4614,#4615,#4616,
#4617,#4618,#4619,#4620,#4621,#4622,#4623,#4624,#4625,#4626,#4627,#4628,
#4629,#4630,#4631,#4632,#4633,#4634,#4635,#4636,#4637,#4638,#4639,#4640,
#4641,#4642,#4643,#4644,#4645,#4646,#4647,#4648,#4649,#4650,#4651,#4652,
#4653,#4654,#4655,#4656,#4657,#4658,#4659,#4660,#4661,#4662,#4663,#4664,
#4665,#4666,#4667,#4668,#4669,#4670,#4671,#4672,#4673,#4674,#4675,#4676,
#4677,#4678,#4679,#4680,#4681,#4682,#4683,#4684,#4685,#4686,#4687,#4688,
#4689,#4690,#4691,#4692,#4693,#4694,#4695,#4696,#4697,#4698,#4699,#4700,
#4701,#4702,#4703,#4704,#4705,#4706,#4707,#4708,#4709,#4710,#4711));
#4826=CLOSED_SHELL('',(#4712,#4713,#4714,#4715,#4716,#4717,#4718,#4719,
#4720,#4721,#4722,#4723,#4724,#4725,#4726,#4727,#4728,#4729,#4730));
#4827=CLOSED_SHELL('',(#4731,#4732,#4733,#4734,#4735,#4736,#4737,#4738,
#4739,#4740,#4741,#4742,#4743,#4744,#4745,#4746,#4747,#4748,#4749));
#4828=CLOSED_SHELL('',(#4750,#4751,#4752,#4753,#4754,#4755,#4756,#4757));
#4829=CLOSED_SHELL('',(#4758,#4759,#4760,#4761,#4762,#4763,#4764,#4765,
#4766,#4767,#4768,#4769,#4770,#4771,#4772,#4773,#4774,#4775));
#4830=CLOSED_SHELL('',(#4776,#4777,#4778,#4779,#4780,#4781,#4782,#4783,
#4784,#4785,#4786,#4787,#4788,#4789,#4790,#4791,#4792,#4793,#4794,#4795,
#4796,#4797,#4798,#4799,#4800,#4801,#4802,#4803,#4804,#4805,#4806,#4807,
#4808,#4809,#4810,#4811,#4812,#4813,#4814,#4815,#4816,#4817,#4818,#4819,
#4820,#4821,#4822,#4823));
#4831=CLOSED_SHELL('',(#4824));
#4832=DERIVED_UNIT_ELEMENT(#4846,1.);
#4833=DERIVED_UNIT_ELEMENT(#19880,-3.);
#4834=DERIVED_UNIT_ELEMENT(#4846,1.);
#4835=DERIVED_UNIT_ELEMENT(#19880,-3.);
#4836=DERIVED_UNIT_ELEMENT(#4846,1.);
#4837=DERIVED_UNIT_ELEMENT(#19880,-3.);
#4838=DERIVED_UNIT_ELEMENT(#4846,1.);
#4839=DERIVED_UNIT_ELEMENT(#19880,-3.);
#4840=DERIVED_UNIT_ELEMENT(#4846,1.);
#4841=DERIVED_UNIT_ELEMENT(#19880,-3.);
#4842=DERIVED_UNIT_ELEMENT(#4846,1.);
#4843=DERIVED_UNIT_ELEMENT(#19880,-3.);
#4844=DERIVED_UNIT_ELEMENT(#4846,1.);
#4845=DERIVED_UNIT_ELEMENT(#19880,-3.);
#4846=(
MASS_UNIT()
NAMED_UNIT(*)
SI_UNIT(.KILO.,.GRAM.)
);
#4847=DERIVED_UNIT((#4832,#4833));
#4848=DERIVED_UNIT((#4834,#4835));
#4849=DERIVED_UNIT((#4836,#4837));
#4850=DERIVED_UNIT((#4838,#4839));
#4851=DERIVED_UNIT((#4840,#4841));
#4852=DERIVED_UNIT((#4842,#4843));
#4853=DERIVED_UNIT((#4844,#4845));
#4854=MEASURE_REPRESENTATION_ITEM('density measure',
POSITIVE_RATIO_MEASURE(7850.),#4847);
#4855=MEASURE_REPRESENTATION_ITEM('density measure',
POSITIVE_RATIO_MEASURE(7750.),#4848);
#4856=MEASURE_REPRESENTATION_ITEM('density measure',
POSITIVE_RATIO_MEASURE(7750.),#4849);
#4857=MEASURE_REPRESENTATION_ITEM('density measure',
POSITIVE_RATIO_MEASURE(7850.),#4850);
#4858=MEASURE_REPRESENTATION_ITEM('density measure',
POSITIVE_RATIO_MEASURE(7850.),#4851);
#4859=MEASURE_REPRESENTATION_ITEM('density measure',
POSITIVE_RATIO_MEASURE(7850.),#4852);
#4860=MEASURE_REPRESENTATION_ITEM('density measure',
POSITIVE_RATIO_MEASURE(7850.),#4853);
#4861=PROPERTY_DEFINITION_REPRESENTATION(#4896,#4875);
#4862=PROPERTY_DEFINITION_REPRESENTATION(#4897,#4876);
#4863=PROPERTY_DEFINITION_REPRESENTATION(#4898,#4877);
#4864=PROPERTY_DEFINITION_REPRESENTATION(#4899,#4878);
#4865=PROPERTY_DEFINITION_REPRESENTATION(#4900,#4879);
#4866=PROPERTY_DEFINITION_REPRESENTATION(#4901,#4880);
#4867=PROPERTY_DEFINITION_REPRESENTATION(#4902,#4881);
#4868=PROPERTY_DEFINITION_REPRESENTATION(#4903,#4882);
#4869=PROPERTY_DEFINITION_REPRESENTATION(#4904,#4883);
#4870=PROPERTY_DEFINITION_REPRESENTATION(#4905,#4884);
#4871=PROPERTY_DEFINITION_REPRESENTATION(#4906,#4885);
#4872=PROPERTY_DEFINITION_REPRESENTATION(#4907,#4886);
#4873=PROPERTY_DEFINITION_REPRESENTATION(#4908,#4887);
#4874=PROPERTY_DEFINITION_REPRESENTATION(#4909,#4888);
#4875=REPRESENTATION('material name',(#4889),#19871);
#4876=REPRESENTATION('density',(#4854),#19871);
#4877=REPRESENTATION('material name',(#4890),#19872);
#4878=REPRESENTATION('density',(#4855),#19872);
#4879=REPRESENTATION('material name',(#4891),#19873);
#4880=REPRESENTATION('density',(#4856),#19873);
#4881=REPRESENTATION('material name',(#4892),#19874);
#4882=REPRESENTATION('density',(#4857),#19874);
#4883=REPRESENTATION('material name',(#4893),#19875);
#4884=REPRESENTATION('density',(#4858),#19875);
#4885=REPRESENTATION('material name',(#4894),#19876);
#4886=REPRESENTATION('density',(#4859),#19876);
#4887=REPRESENTATION('material name',(#4895),#19877);
#4888=REPRESENTATION('density',(#4860),#19877);
#4889=DESCRIPTIVE_REPRESENTATION_ITEM('Steel','Steel');
#4890=DESCRIPTIVE_REPRESENTATION_ITEM('Steel Grade 2, Plain',
'Steel Grade 2, Plain');
#4891=DESCRIPTIVE_REPRESENTATION_ITEM('Steel Grade 2, Plain',
'Steel Grade 2, Plain');
#4892=DESCRIPTIVE_REPRESENTATION_ITEM('Steel','Steel');
#4893=DESCRIPTIVE_REPRESENTATION_ITEM('Steel','Steel');
#4894=DESCRIPTIVE_REPRESENTATION_ITEM('Steel','Steel');
#4895=DESCRIPTIVE_REPRESENTATION_ITEM('Steel','Steel');
#4896=PROPERTY_DEFINITION('material property','material name',#19916);
#4897=PROPERTY_DEFINITION('material property','density of part',#19916);
#4898=PROPERTY_DEFINITION('material property','material name',#19917);
#4899=PROPERTY_DEFINITION('material property','density of part',#19917);
#4900=PROPERTY_DEFINITION('material property','material name',#19918);
#4901=PROPERTY_DEFINITION('material property','density of part',#19918);
#4902=PROPERTY_DEFINITION('material property','material name',#19919);
#4903=PROPERTY_DEFINITION('material property','density of part',#19919);
#4904=PROPERTY_DEFINITION('material property','material name',#19920);
#4905=PROPERTY_DEFINITION('material property','density of part',#19920);
#4906=PROPERTY_DEFINITION('material property','material name',#19921);
#4907=PROPERTY_DEFINITION('material property','density of part',#19921);
#4908=PROPERTY_DEFINITION('material property','material name',#19922);
#4909=PROPERTY_DEFINITION('material property','density of part',#19922);
#4910=AXIS2_PLACEMENT_3D('',#6817,#5427,#5428);
#4911=AXIS2_PLACEMENT_3D('',#6818,#5429,#5430);
#4912=AXIS2_PLACEMENT_3D('',#6819,#5431,#5432);
#4913=AXIS2_PLACEMENT_3D('',#6821,#5433,#5434);
#4914=AXIS2_PLACEMENT_3D('',#6824,#5436,#5437);
#4915=AXIS2_PLACEMENT_3D('',#6825,#5438,#5439);
#4916=AXIS2_PLACEMENT_3D('',#6828,#5440,#5441);
#4917=AXIS2_PLACEMENT_3D('',#6832,#5443,#5444);
#4918=AXIS2_PLACEMENT_3D('',#6834,#5446,#5447);
#4919=AXIS2_PLACEMENT_3D('',#6840,#5451,#5452);
#4920=AXIS2_PLACEMENT_3D('',#6843,#5453,#5454);
#4921=AXIS2_PLACEMENT_3D('',#6847,#5456,#5457);
#4922=AXIS2_PLACEMENT_3D('',#6849,#5459,#5460);
#4923=AXIS2_PLACEMENT_3D('',#6855,#5464,#5465);
#4924=AXIS2_PLACEMENT_3D('',#6858,#5466,#5467);
#4925=AXIS2_PLACEMENT_3D('',#6862,#5469,#5470);
#4926=AXIS2_PLACEMENT_3D('',#6864,#5472,#5473);
#4927=AXIS2_PLACEMENT_3D('',#6870,#5477,#5478);
#4928=AXIS2_PLACEMENT_3D('',#6873,#5479,#5480);
#4929=AXIS2_PLACEMENT_3D('',#6877,#5482,#5483);
#4930=AXIS2_PLACEMENT_3D('',#6879,#5485,#5486);
#4931=AXIS2_PLACEMENT_3D('',#6885,#5490,#5491);
#4932=AXIS2_PLACEMENT_3D('',#6888,#5492,#5493);
#4933=AXIS2_PLACEMENT_3D('',#6892,#5495,#5496);
#4934=AXIS2_PLACEMENT_3D('',#6894,#5498,#5499);
#4935=AXIS2_PLACEMENT_3D('',#6900,#5503,#5504);
#4936=AXIS2_PLACEMENT_3D('',#6903,#5505,#5506);
#4937=AXIS2_PLACEMENT_3D('',#6907,#5508,#5509);
#4938=AXIS2_PLACEMENT_3D('',#6909,#5511,#5512);
#4939=AXIS2_PLACEMENT_3D('',#6915,#5516,#5517);
#4940=AXIS2_PLACEMENT_3D('',#6918,#5518,#5519);
#4941=AXIS2_PLACEMENT_3D('',#6922,#5521,#5522);
#4942=AXIS2_PLACEMENT_3D('',#6924,#5524,#5525);
#4943=AXIS2_PLACEMENT_3D('',#6930,#5529,#5530);
#4944=AXIS2_PLACEMENT_3D('',#6933,#5531,#5532);
#4945=AXIS2_PLACEMENT_3D('',#6937,#5534,#5535);
#4946=AXIS2_PLACEMENT_3D('',#6939,#5537,#5538);
#4947=AXIS2_PLACEMENT_3D('',#6945,#5542,#5543);
#4948=AXIS2_PLACEMENT_3D('',#6948,#5544,#5545);
#4949=AXIS2_PLACEMENT_3D('',#6952,#5547,#5548);
#4950=AXIS2_PLACEMENT_3D('',#6954,#5550,#5551);
#4951=AXIS2_PLACEMENT_3D('',#6960,#5555,#5556);
#4952=AXIS2_PLACEMENT_3D('',#6963,#5557,#5558);
#4953=AXIS2_PLACEMENT_3D('',#6967,#5560,#5561);
#4954=AXIS2_PLACEMENT_3D('',#6969,#5563,#5564);
#4955=AXIS2_PLACEMENT_3D('',#6975,#5568,#5569);
#4956=AXIS2_PLACEMENT_3D('',#6978,#5570,#5571);
#4957=AXIS2_PLACEMENT_3D('',#6982,#5573,#5574);
#4958=AXIS2_PLACEMENT_3D('',#6984,#5576,#5577);
#4959=AXIS2_PLACEMENT_3D('',#6990,#5581,#5582);
#4960=AXIS2_PLACEMENT_3D('',#6993,#5583,#5584);
#4961=AXIS2_PLACEMENT_3D('',#6997,#5586,#5587);
#4962=AXIS2_PLACEMENT_3D('',#6999,#5589,#5590);
#4963=AXIS2_PLACEMENT_3D('',#7005,#5594,#5595);
#4964=AXIS2_PLACEMENT_3D('',#7008,#5596,#5597);
#4965=AXIS2_PLACEMENT_3D('',#7012,#5599,#5600);
#4966=AXIS2_PLACEMENT_3D('',#7014,#5602,#5603);
#4967=AXIS2_PLACEMENT_3D('',#7020,#5607,#5608);
#4968=AXIS2_PLACEMENT_3D('',#7023,#5609,#5610);
#4969=AXIS2_PLACEMENT_3D('',#7027,#5612,#5613);
#4970=AXIS2_PLACEMENT_3D('',#7029,#5615,#5616);
#4971=AXIS2_PLACEMENT_3D('',#7035,#5620,#5621);
#4972=AXIS2_PLACEMENT_3D('',#7038,#5622,#5623);
#4973=AXIS2_PLACEMENT_3D('',#7042,#5625,#5626);
#4974=AXIS2_PLACEMENT_3D('',#7044,#5628,#5629);
#4975=AXIS2_PLACEMENT_3D('',#7050,#5633,#5634);
#4976=AXIS2_PLACEMENT_3D('',#7053,#5635,#5636);
#4977=AXIS2_PLACEMENT_3D('',#7057,#5638,#5639);
#4978=AXIS2_PLACEMENT_3D('',#7059,#5641,#5642);
#4979=AXIS2_PLACEMENT_3D('',#7065,#5646,#5647);
#4980=AXIS2_PLACEMENT_3D('',#7068,#5648,#5649);
#4981=AXIS2_PLACEMENT_3D('',#7072,#5651,#5652);
#4982=AXIS2_PLACEMENT_3D('',#7074,#5654,#5655);
#4983=AXIS2_PLACEMENT_3D('',#7080,#5659,#5660);
#4984=AXIS2_PLACEMENT_3D('',#7083,#5661,#5662);
#4985=AXIS2_PLACEMENT_3D('',#7087,#5664,#5665);
#4986=AXIS2_PLACEMENT_3D('',#7089,#5667,#5668);
#4987=AXIS2_PLACEMENT_3D('',#7095,#5672,#5673);
#4988=AXIS2_PLACEMENT_3D('',#7098,#5674,#5675);
#4989=AXIS2_PLACEMENT_3D('',#7102,#5677,#5678);
#4990=AXIS2_PLACEMENT_3D('',#7104,#5680,#5681);
#4991=AXIS2_PLACEMENT_3D('',#7110,#5685,#5686);
#4992=AXIS2_PLACEMENT_3D('',#7113,#5687,#5688);
#4993=AXIS2_PLACEMENT_3D('',#7117,#5690,#5691);
#4994=AXIS2_PLACEMENT_3D('',#7119,#5693,#5694);
#4995=AXIS2_PLACEMENT_3D('',#7125,#5698,#5699);
#4996=AXIS2_PLACEMENT_3D('',#7128,#5700,#5701);
#4997=AXIS2_PLACEMENT_3D('',#7132,#5703,#5704);
#4998=AXIS2_PLACEMENT_3D('',#7134,#5706,#5707);
#4999=AXIS2_PLACEMENT_3D('',#7140,#5711,#5712);
#5000=AXIS2_PLACEMENT_3D('',#7143,#5713,#5714);
#5001=AXIS2_PLACEMENT_3D('',#7147,#5716,#5717);
#5002=AXIS2_PLACEMENT_3D('',#7149,#5719,#5720);
#5003=AXIS2_PLACEMENT_3D('',#7155,#5724,#5725);
#5004=AXIS2_PLACEMENT_3D('',#7158,#5726,#5727);
#5005=AXIS2_PLACEMENT_3D('',#7162,#5729,#5730);
#5006=AXIS2_PLACEMENT_3D('',#7164,#5732,#5733);
#5007=AXIS2_PLACEMENT_3D('',#7170,#5737,#5738);
#5008=AXIS2_PLACEMENT_3D('',#7173,#5739,#5740);
#5009=AXIS2_PLACEMENT_3D('',#7177,#5742,#5743);
#5010=AXIS2_PLACEMENT_3D('',#7179,#5745,#5746);
#5011=AXIS2_PLACEMENT_3D('',#7185,#5750,#5751);
#5012=AXIS2_PLACEMENT_3D('',#7188,#5752,#5753);
#5013=AXIS2_PLACEMENT_3D('',#7192,#5755,#5756);
#5014=AXIS2_PLACEMENT_3D('',#7194,#5758,#5759);
#5015=AXIS2_PLACEMENT_3D('',#7200,#5763,#5764);
#5016=AXIS2_PLACEMENT_3D('',#7203,#5765,#5766);
#5017=AXIS2_PLACEMENT_3D('',#7207,#5768,#5769);
#5018=AXIS2_PLACEMENT_3D('',#7209,#5771,#5772);
#5019=AXIS2_PLACEMENT_3D('',#7215,#5776,#5777);
#5020=AXIS2_PLACEMENT_3D('',#7218,#5778,#5779);
#5021=AXIS2_PLACEMENT_3D('',#7222,#5781,#5782);
#5022=AXIS2_PLACEMENT_3D('',#7224,#5784,#5785);
#5023=AXIS2_PLACEMENT_3D('',#7230,#5789,#5790);
#5024=AXIS2_PLACEMENT_3D('',#7233,#5791,#5792);
#5025=AXIS2_PLACEMENT_3D('',#7237,#5794,#5795);
#5026=AXIS2_PLACEMENT_3D('',#7239,#5797,#5798);
#5027=AXIS2_PLACEMENT_3D('',#7245,#5802,#5803);
#5028=AXIS2_PLACEMENT_3D('',#7248,#5804,#5805);
#5029=AXIS2_PLACEMENT_3D('',#7252,#5807,#5808);
#5030=AXIS2_PLACEMENT_3D('',#7254,#5810,#5811);
#5031=AXIS2_PLACEMENT_3D('',#7260,#5815,#5816);
#5032=AXIS2_PLACEMENT_3D('',#7263,#5817,#5818);
#5033=AXIS2_PLACEMENT_3D('',#7267,#5820,#5821);
#5034=AXIS2_PLACEMENT_3D('',#7269,#5823,#5824);
#5035=AXIS2_PLACEMENT_3D('',#7275,#5828,#5829);
#5036=AXIS2_PLACEMENT_3D('',#7278,#5830,#5831);
#5037=AXIS2_PLACEMENT_3D('',#7282,#5833,#5834);
#5038=AXIS2_PLACEMENT_3D('',#7284,#5836,#5837);
#5039=AXIS2_PLACEMENT_3D('',#7290,#5841,#5842);
#5040=AXIS2_PLACEMENT_3D('',#7293,#5843,#5844);
#5041=AXIS2_PLACEMENT_3D('',#7297,#5846,#5847);
#5042=AXIS2_PLACEMENT_3D('',#7299,#5849,#5850);
#5043=AXIS2_PLACEMENT_3D('',#7305,#5854,#5855);
#5044=AXIS2_PLACEMENT_3D('',#7308,#5856,#5857);
#5045=AXIS2_PLACEMENT_3D('',#7312,#5859,#5860);
#5046=AXIS2_PLACEMENT_3D('',#7314,#5862,#5863);
#5047=AXIS2_PLACEMENT_3D('',#7320,#5867,#5868);
#5048=AXIS2_PLACEMENT_3D('',#7323,#5869,#5870);
#5049=AXIS2_PLACEMENT_3D('',#7327,#5872,#5873);
#5050=AXIS2_PLACEMENT_3D('',#7329,#5875,#5876);
#5051=AXIS2_PLACEMENT_3D('',#7335,#5880,#5881);
#5052=AXIS2_PLACEMENT_3D('',#7338,#5882,#5883);
#5053=AXIS2_PLACEMENT_3D('',#7342,#5885,#5886);
#5054=AXIS2_PLACEMENT_3D('',#7344,#5888,#5889);
#5055=AXIS2_PLACEMENT_3D('',#7350,#5893,#5894);
#5056=AXIS2_PLACEMENT_3D('',#7353,#5895,#5896);
#5057=AXIS2_PLACEMENT_3D('',#7357,#5898,#5899);
#5058=AXIS2_PLACEMENT_3D('',#7359,#5901,#5902);
#5059=AXIS2_PLACEMENT_3D('',#7365,#5906,#5907);
#5060=AXIS2_PLACEMENT_3D('',#7368,#5908,#5909);
#5061=AXIS2_PLACEMENT_3D('',#7372,#5911,#5912);
#5062=AXIS2_PLACEMENT_3D('',#7374,#5914,#5915);
#5063=AXIS2_PLACEMENT_3D('',#7380,#5919,#5920);
#5064=AXIS2_PLACEMENT_3D('',#7383,#5921,#5922);
#5065=AXIS2_PLACEMENT_3D('',#7387,#5924,#5925);
#5066=AXIS2_PLACEMENT_3D('',#7389,#5927,#5928);
#5067=AXIS2_PLACEMENT_3D('',#7689,#5933,#5934);
#5068=AXIS2_PLACEMENT_3D('',#7691,#5935,#5936);
#5069=AXIS2_PLACEMENT_3D('',#7693,#5937,#5938);
#5070=AXIS2_PLACEMENT_3D('',#8283,#5941,#5942);
#5071=AXIS2_PLACEMENT_3D('',#8285,#5943,#5944);
#5072=AXIS2_PLACEMENT_3D('',#8287,#5945,#5946);
#5073=AXIS2_PLACEMENT_3D('',#8883,#5949,#5950);
#5074=AXIS2_PLACEMENT_3D('',#8885,#5951,#5952);
#5075=AXIS2_PLACEMENT_3D('',#8887,#5953,#5954);
#5076=AXIS2_PLACEMENT_3D('',#9477,#5957,#5958);
#5077=AXIS2_PLACEMENT_3D('',#9479,#5959,#5960);
#5078=AXIS2_PLACEMENT_3D('',#9481,#5961,#5962);
#5079=AXIS2_PLACEMENT_3D('',#10071,#5965,#5966);
#5080=AXIS2_PLACEMENT_3D('',#10073,#5967,#5968);
#5081=AXIS2_PLACEMENT_3D('',#10075,#5969,#5970);
#5082=AXIS2_PLACEMENT_3D('',#10665,#5973,#5974);
#5083=AXIS2_PLACEMENT_3D('',#10667,#5975,#5976);
#5084=AXIS2_PLACEMENT_3D('',#10669,#5977,#5978);
#5085=AXIS2_PLACEMENT_3D('',#11259,#5981,#5982);
#5086=AXIS2_PLACEMENT_3D('',#11261,#5983,#5984);
#5087=AXIS2_PLACEMENT_3D('',#11263,#5985,#5986);
#5088=AXIS2_PLACEMENT_3D('',#11853,#5989,#5990);
#5089=AXIS2_PLACEMENT_3D('',#11855,#5991,#5992);
#5090=AXIS2_PLACEMENT_3D('',#11857,#5993,#5994);
#5091=AXIS2_PLACEMENT_3D('',#12447,#5997,#5998);
#5092=AXIS2_PLACEMENT_3D('',#12449,#5999,#6000);
#5093=AXIS2_PLACEMENT_3D('',#12451,#6001,#6002);
#5094=AXIS2_PLACEMENT_3D('',#13041,#6005,#6006);
#5095=AXIS2_PLACEMENT_3D('',#13043,#6007,#6008);
#5096=AXIS2_PLACEMENT_3D('',#13045,#6009,#6010);
#5097=AXIS2_PLACEMENT_3D('',#13635,#6013,#6014);
#5098=AXIS2_PLACEMENT_3D('',#13637,#6015,#6016);
#5099=AXIS2_PLACEMENT_3D('',#13639,#6017,#6018);
#5100=AXIS2_PLACEMENT_3D('',#14229,#6021,#6022);
#5101=AXIS2_PLACEMENT_3D('',#14231,#6023,#6024);
#5102=AXIS2_PLACEMENT_3D('',#14233,#6025,#6026);
#5103=AXIS2_PLACEMENT_3D('',#14823,#6029,#6030);
#5104=AXIS2_PLACEMENT_3D('',#14825,#6031,#6032);
#5105=AXIS2_PLACEMENT_3D('',#14827,#6033,#6034);
#5106=AXIS2_PLACEMENT_3D('',#15417,#6037,#6038);
#5107=AXIS2_PLACEMENT_3D('',#15419,#6039,#6040);
#5108=AXIS2_PLACEMENT_3D('',#15421,#6041,#6042);
#5109=AXIS2_PLACEMENT_3D('',#16011,#6045,#6046);
#5110=AXIS2_PLACEMENT_3D('',#16013,#6047,#6048);
#5111=AXIS2_PLACEMENT_3D('',#16015,#6049,#6050);
#5112=AXIS2_PLACEMENT_3D('',#16605,#6053,#6054);
#5113=AXIS2_PLACEMENT_3D('',#16607,#6055,#6056);
#5114=AXIS2_PLACEMENT_3D('',#16609,#6057,#6058);
#5115=AXIS2_PLACEMENT_3D('',#17214,#6061,#6062);
#5116=AXIS2_PLACEMENT_3D('',#17216,#6063,#6064);
#5117=AXIS2_PLACEMENT_3D('',#17218,#6065,#6066);
#5118=AXIS2_PLACEMENT_3D('',#17808,#6069,#6070);
#5119=AXIS2_PLACEMENT_3D('',#17810,#6071,#6072);
#5120=AXIS2_PLACEMENT_3D('',#17812,#6073,#6074);
#5121=AXIS2_PLACEMENT_3D('',#18402,#6077,#6078);
#5122=AXIS2_PLACEMENT_3D('',#18404,#6079,#6080);
#5123=AXIS2_PLACEMENT_3D('',#18406,#6081,#6082);
#5124=AXIS2_PLACEMENT_3D('',#18702,#6084,#6085);
#5125=AXIS2_PLACEMENT_3D('',#18703,#6086,#6087);
#5126=AXIS2_PLACEMENT_3D('',#18704,#6088,#6089);
#5127=AXIS2_PLACEMENT_3D('',#18705,#6090,#6091);
#5128=AXIS2_PLACEMENT_3D('',#18706,#6092,#6093);
#5129=AXIS2_PLACEMENT_3D('',#18707,#6094,#6095);
#5130=AXIS2_PLACEMENT_3D('',#18708,#6096,#6097);
#5131=AXIS2_PLACEMENT_3D('',#18709,#6098,#6099);
#5132=AXIS2_PLACEMENT_3D('',#18710,#6100,#6101);
#5133=AXIS2_PLACEMENT_3D('',#18711,#6102,#6103);
#5134=AXIS2_PLACEMENT_3D('',#18712,#6104,#6105);
#5135=AXIS2_PLACEMENT_3D('',#18713,#6106,#6107);
#5136=AXIS2_PLACEMENT_3D('',#18714,#6108,#6109);
#5137=AXIS2_PLACEMENT_3D('',#18715,#6110,#6111);
#5138=AXIS2_PLACEMENT_3D('',#18716,#6112,#6113);
#5139=AXIS2_PLACEMENT_3D('',#18717,#6114,#6115);
#5140=AXIS2_PLACEMENT_3D('',#18718,#6116,#6117);
#5141=AXIS2_PLACEMENT_3D('',#18719,#6118,#6119);
#5142=AXIS2_PLACEMENT_3D('',#18721,#6120,#6121);
#5143=AXIS2_PLACEMENT_3D('',#18723,#6122,#6123);
#5144=AXIS2_PLACEMENT_3D('',#18802,#6125,#6126);
#5145=AXIS2_PLACEMENT_3D('',#18881,#6128,#6129);
#5146=AXIS2_PLACEMENT_3D('',#18882,#6130,#6131);
#5147=AXIS2_PLACEMENT_3D('',#18883,#6132,#6133);
#5148=AXIS2_PLACEMENT_3D('',#18884,#6134,#6135);
#5149=AXIS2_PLACEMENT_3D('',#18886,#6136,#6137);
#5150=AXIS2_PLACEMENT_3D('',#18888,#6138,#6139);
#5151=AXIS2_PLACEMENT_3D('',#18963,#6141,#6142);
#5152=AXIS2_PLACEMENT_3D('',#19035,#6144,#6145);
#5153=AXIS2_PLACEMENT_3D('',#19036,#6146,#6147);
#5154=AXIS2_PLACEMENT_3D('',#19037,#6148,#6149);
#5155=AXIS2_PLACEMENT_3D('',#19038,#6150,#6151);
#5156=AXIS2_PLACEMENT_3D('',#19039,#6152,#6153);
#5157=AXIS2_PLACEMENT_3D('',#19040,#6154,#6155);
#5158=AXIS2_PLACEMENT_3D('',#19041,#6156,#6157);
#5159=AXIS2_PLACEMENT_3D('',#19042,#6158,#6159);
#5160=AXIS2_PLACEMENT_3D('',#19043,#6160,#6161);
#5161=AXIS2_PLACEMENT_3D('',#19044,#6162,#6163);
#5162=AXIS2_PLACEMENT_3D('',#19045,#6164,#6165);
#5163=AXIS2_PLACEMENT_3D('',#19046,#6166,#6167);
#5164=AXIS2_PLACEMENT_3D('',#19047,#6168,#6169);
#5165=AXIS2_PLACEMENT_3D('',#19048,#6170,#6171);
#5166=AXIS2_PLACEMENT_3D('',#19049,#6172,#6173);
#5167=AXIS2_PLACEMENT_3D('',#19050,#6174,#6175);
#5168=AXIS2_PLACEMENT_3D('',#19051,#6176,#6177);
#5169=AXIS2_PLACEMENT_3D('',#19052,#6178,#6179);
#5170=AXIS2_PLACEMENT_3D('',#19053,#6180,#6181);
#5171=AXIS2_PLACEMENT_3D('',#19054,#6182,#6183);
#5172=AXIS2_PLACEMENT_3D('',#19055,#6184,#6185);
#5173=AXIS2_PLACEMENT_3D('',#19057,#6187,#6188);
#5174=AXIS2_PLACEMENT_3D('',#19058,#6189,#6190);
#5175=AXIS2_PLACEMENT_3D('',#19059,#6191,#6192);
#5176=AXIS2_PLACEMENT_3D('',#19060,#6193,#6194);
#5177=AXIS2_PLACEMENT_3D('',#19061,#6195,#6196);
#5178=AXIS2_PLACEMENT_3D('',#19062,#6197,#6198);
#5179=AXIS2_PLACEMENT_3D('',#19063,#6199,#6200);
#5180=AXIS2_PLACEMENT_3D('',#19064,#6201,#6202);
#5181=AXIS2_PLACEMENT_3D('',#19065,#6203,#6204);
#5182=AXIS2_PLACEMENT_3D('',#19066,#6205,#6206);
#5183=AXIS2_PLACEMENT_3D('',#19067,#6207,#6208);
#5184=AXIS2_PLACEMENT_3D('',#19068,#6209,#6210);
#5185=AXIS2_PLACEMENT_3D('',#19069,#6211,#6212);
#5186=AXIS2_PLACEMENT_3D('',#19070,#6213,#6214);
#5187=AXIS2_PLACEMENT_3D('',#19071,#6215,#6216);
#5188=AXIS2_PLACEMENT_3D('',#19072,#6217,#6218);
#5189=AXIS2_PLACEMENT_3D('',#19073,#6219,#6220);
#5190=AXIS2_PLACEMENT_3D('',#19074,#6221,#6222);
#5191=AXIS2_PLACEMENT_3D('',#19075,#6223,#6224);
#5192=AXIS2_PLACEMENT_3D('',#19077,#6226,#6227);
#5193=AXIS2_PLACEMENT_3D('',#19079,#6229,#6230);
#5194=AXIS2_PLACEMENT_3D('',#19082,#6233,#6234);
#5195=AXIS2_PLACEMENT_3D('',#19235,#6237,#6238);
#5196=AXIS2_PLACEMENT_3D('',#19387,#6240,#6241);
#5197=AXIS2_PLACEMENT_3D('',#19388,#6242,#6243);
#5198=AXIS2_PLACEMENT_3D('',#19389,#6244,#6245);
#5199=AXIS2_PLACEMENT_3D('',#19391,#6246,#6247);
#5200=AXIS2_PLACEMENT_3D('',#19394,#6249,#6250);
#5201=AXIS2_PLACEMENT_3D('',#19395,#6251,#6252);
#5202=AXIS2_PLACEMENT_3D('',#19397,#6253,#6254);
#5203=AXIS2_PLACEMENT_3D('',#19399,#6255,#6256);
#5204=AXIS2_PLACEMENT_3D('',#19400,#6257,#6258);
#5205=AXIS2_PLACEMENT_3D('',#19401,#6259,#6260);
#5206=AXIS2_PLACEMENT_3D('',#19403,#6261,#6262);
#5207=AXIS2_PLACEMENT_3D('',#19405,#6264,#6265);
#5208=AXIS2_PLACEMENT_3D('',#19407,#6267,#6268);
#5209=AXIS2_PLACEMENT_3D('',#19414,#6272,#6273);
#5210=AXIS2_PLACEMENT_3D('',#19418,#6276,#6277);
#5211=AXIS2_PLACEMENT_3D('',#19422,#6280,#6281);
#5212=AXIS2_PLACEMENT_3D('',#19426,#6284,#6285);
#5213=AXIS2_PLACEMENT_3D('',#19430,#6288,#6289);
#5214=AXIS2_PLACEMENT_3D('',#19432,#6291,#6292);
#5215=AXIS2_PLACEMENT_3D('',#19438,#6296,#6297);
#5216=AXIS2_PLACEMENT_3D('',#19442,#6300,#6301);
#5217=AXIS2_PLACEMENT_3D('',#19446,#6304,#6305);
#5218=AXIS2_PLACEMENT_3D('',#19450,#6308,#6309);
#5219=AXIS2_PLACEMENT_3D('',#19454,#6312,#6313);
#5220=AXIS2_PLACEMENT_3D('',#19456,#6315,#6316);
#5221=AXIS2_PLACEMENT_3D('',#19458,#6317,#6318);
#5222=AXIS2_PLACEMENT_3D('',#19459,#6319,#6320);
#5223=AXIS2_PLACEMENT_3D('',#19461,#6322,#6323);
#5224=AXIS2_PLACEMENT_3D('',#19462,#6324,#6325);
#5225=AXIS2_PLACEMENT_3D('',#19463,#6326,#6327);
#5226=AXIS2_PLACEMENT_3D('',#19465,#6328,#6329);
#5227=AXIS2_PLACEMENT_3D('',#19468,#6331,#6332);
#5228=AXIS2_PLACEMENT_3D('',#19469,#6333,#6334);
#5229=AXIS2_PLACEMENT_3D('',#19471,#6335,#6336);
#5230=AXIS2_PLACEMENT_3D('',#19473,#6337,#6338);
#5231=AXIS2_PLACEMENT_3D('',#19474,#6339,#6340);
#5232=AXIS2_PLACEMENT_3D('',#19475,#6341,#6342);
#5233=AXIS2_PLACEMENT_3D('',#19477,#6343,#6344);
#5234=AXIS2_PLACEMENT_3D('',#19479,#6346,#6347);
#5235=AXIS2_PLACEMENT_3D('',#19481,#6349,#6350);
#5236=AXIS2_PLACEMENT_3D('',#19488,#6354,#6355);
#5237=AXIS2_PLACEMENT_3D('',#19492,#6358,#6359);
#5238=AXIS2_PLACEMENT_3D('',#19496,#6362,#6363);
#5239=AXIS2_PLACEMENT_3D('',#19500,#6366,#6367);
#5240=AXIS2_PLACEMENT_3D('',#19504,#6370,#6371);
#5241=AXIS2_PLACEMENT_3D('',#19506,#6373,#6374);
#5242=AXIS2_PLACEMENT_3D('',#19512,#6378,#6379);
#5243=AXIS2_PLACEMENT_3D('',#19516,#6382,#6383);
#5244=AXIS2_PLACEMENT_3D('',#19520,#6386,#6387);
#5245=AXIS2_PLACEMENT_3D('',#19524,#6390,#6391);
#5246=AXIS2_PLACEMENT_3D('',#19528,#6394,#6395);
#5247=AXIS2_PLACEMENT_3D('',#19530,#6397,#6398);
#5248=AXIS2_PLACEMENT_3D('',#19532,#6399,#6400);
#5249=AXIS2_PLACEMENT_3D('',#19533,#6401,#6402);
#5250=AXIS2_PLACEMENT_3D('',#19535,#6404,#6405);
#5251=AXIS2_PLACEMENT_3D('',#19536,#6406,#6407);
#5252=AXIS2_PLACEMENT_3D('',#19537,#6408,#6409);
#5253=AXIS2_PLACEMENT_3D('',#19539,#6410,#6411);
#5254=AXIS2_PLACEMENT_3D('',#19542,#6413,#6414);
#5255=AXIS2_PLACEMENT_3D('',#19543,#6415,#6416);
#5256=AXIS2_PLACEMENT_3D('',#19545,#6417,#6418);
#5257=AXIS2_PLACEMENT_3D('',#19546,#6419,#6420);
#5258=AXIS2_PLACEMENT_3D('',#19548,#6421,#6422);
#5259=AXIS2_PLACEMENT_3D('',#19550,#6423,#6424);
#5260=AXIS2_PLACEMENT_3D('',#19551,#6425,#6426);
#5261=AXIS2_PLACEMENT_3D('',#19552,#6427,#6428);
#5262=AXIS2_PLACEMENT_3D('',#19554,#6430,#6431);
#5263=AXIS2_PLACEMENT_3D('',#19556,#6432,#6433);
#5264=AXIS2_PLACEMENT_3D('',#19557,#6434,#6435);
#5265=AXIS2_PLACEMENT_3D('',#19559,#6436,#6437);
#5266=AXIS2_PLACEMENT_3D('',#19561,#6439,#6440);
#5267=AXIS2_PLACEMENT_3D('',#19562,#6441,#6442);
#5268=AXIS2_PLACEMENT_3D('',#19563,#6443,#6444);
#5269=AXIS2_PLACEMENT_3D('',#19564,#6445,#6446);
#5270=AXIS2_PLACEMENT_3D('',#19566,#6447,#6448);
#5271=AXIS2_PLACEMENT_3D('',#19568,#6449,#6450);
#5272=AXIS2_PLACEMENT_3D('',#19569,#6451,#6452);
#5273=AXIS2_PLACEMENT_3D('',#19570,#6453,#6454);
#5274=AXIS2_PLACEMENT_3D('',#19573,#6456,#6457);
#5275=AXIS2_PLACEMENT_3D('',#19574,#6458,#6459);
#5276=AXIS2_PLACEMENT_3D('',#19576,#6460,#6461);
#5277=AXIS2_PLACEMENT_3D('',#19577,#6462,#6463);
#5278=AXIS2_PLACEMENT_3D('',#19579,#6464,#6465);
#5279=AXIS2_PLACEMENT_3D('',#19581,#6466,#6467);
#5280=AXIS2_PLACEMENT_3D('',#19582,#6468,#6469);
#5281=AXIS2_PLACEMENT_3D('',#19583,#6470,#6471);
#5282=AXIS2_PLACEMENT_3D('',#19585,#6472,#6473);
#5283=AXIS2_PLACEMENT_3D('',#19586,#6474,#6475);
#5284=AXIS2_PLACEMENT_3D('',#19588,#6476,#6477);
#5285=AXIS2_PLACEMENT_3D('',#19590,#6479,#6480);
#5286=AXIS2_PLACEMENT_3D('',#19592,#6481,#6482);
#5287=AXIS2_PLACEMENT_3D('',#19593,#6483,#6484);
#5288=AXIS2_PLACEMENT_3D('',#19594,#6485,#6486);
#5289=AXIS2_PLACEMENT_3D('',#19597,#6488,#6489);
#5290=AXIS2_PLACEMENT_3D('',#19598,#6490,#6491);
#5291=AXIS2_PLACEMENT_3D('',#19599,#6492,#6493);
#5292=AXIS2_PLACEMENT_3D('',#19601,#6494,#6495);
#5293=AXIS2_PLACEMENT_3D('',#19603,#6497,#6498);
#5294=AXIS2_PLACEMENT_3D('',#19605,#6499,#6500);
#5295=AXIS2_PLACEMENT_3D('',#19606,#6501,#6502);
#5296=AXIS2_PLACEMENT_3D('',#19607,#6503,#6504);
#5297=AXIS2_PLACEMENT_3D('',#19609,#6505,#6506);
#5298=AXIS2_PLACEMENT_3D('',#19610,#6507,#6508);
#5299=AXIS2_PLACEMENT_3D('',#19612,#6509,#6510);
#5300=AXIS2_PLACEMENT_3D('',#19614,#6512,#6513);
#5301=AXIS2_PLACEMENT_3D('',#19616,#6514,#6515);
#5302=AXIS2_PLACEMENT_3D('',#19617,#6516,#6517);
#5303=AXIS2_PLACEMENT_3D('',#19619,#6518,#6519);
#5304=AXIS2_PLACEMENT_3D('',#19621,#6521,#6522);
#5305=AXIS2_PLACEMENT_3D('',#19623,#6523,#6524);
#5306=AXIS2_PLACEMENT_3D('',#19624,#6525,#6526);
#5307=AXIS2_PLACEMENT_3D('',#19626,#6527,#6528);
#5308=AXIS2_PLACEMENT_3D('',#19628,#6530,#6531);
#5309=AXIS2_PLACEMENT_3D('',#19629,#6532,#6533);
#5310=AXIS2_PLACEMENT_3D('',#19630,#6534,#6535);
#5311=AXIS2_PLACEMENT_3D('',#19633,#6536,#6537);
#5312=AXIS2_PLACEMENT_3D('',#19637,#6539,#6540);
#5313=AXIS2_PLACEMENT_3D('',#19639,#6542,#6543);
#5314=AXIS2_PLACEMENT_3D('',#19642,#6544,#6545);
#5315=AXIS2_PLACEMENT_3D('',#19643,#6546,#6547);
#5316=AXIS2_PLACEMENT_3D('',#19645,#6548,#6549);
#5317=AXIS2_PLACEMENT_3D('',#19646,#6550,#6551);
#5318=AXIS2_PLACEMENT_3D('',#19647,#6552,#6553);
#5319=AXIS2_PLACEMENT_3D('',#19648,#6554,#6555);
#5320=AXIS2_PLACEMENT_3D('',#19649,#6556,#6557);
#5321=AXIS2_PLACEMENT_3D('',#19651,#6558,#6559);
#5322=AXIS2_PLACEMENT_3D('',#19655,#6561,#6562);
#5323=AXIS2_PLACEMENT_3D('',#19657,#6564,#6565);
#5324=AXIS2_PLACEMENT_3D('',#19658,#6566,#6567);
#5325=AXIS2_PLACEMENT_3D('',#19659,#6568,#6569);
#5326=AXIS2_PLACEMENT_3D('',#19669,#6575,#6576);
#5327=AXIS2_PLACEMENT_3D('',#19671,#6577,#6578);
#5328=AXIS2_PLACEMENT_3D('',#19673,#6580,#6581);
#5329=AXIS2_PLACEMENT_3D('',#19675,#6582,#6583);
#5330=AXIS2_PLACEMENT_3D('',#19679,#6585,#6586);
#5331=AXIS2_PLACEMENT_3D('',#19682,#6588,#6589);
#5332=AXIS2_PLACEMENT_3D('',#19683,#6590,#6591);
#5333=AXIS2_PLACEMENT_3D('',#19685,#6592,#6593);
#5334=AXIS2_PLACEMENT_3D('',#19687,#6595,#6596);
#5335=AXIS2_PLACEMENT_3D('',#19695,#6601,#6602);
#5336=AXIS2_PLACEMENT_3D('',#19697,#6603,#6604);
#5337=AXIS2_PLACEMENT_3D('',#19698,#6605,#6606);
#5338=AXIS2_PLACEMENT_3D('',#19699,#6607,#6608);
#5339=AXIS2_PLACEMENT_3D('',#19701,#6609,#6610);
#5340=AXIS2_PLACEMENT_3D('',#19703,#6612,#6613);
#5341=AXIS2_PLACEMENT_3D('',#19704,#6614,#6615);
#5342=AXIS2_PLACEMENT_3D('',#19705,#6616,#6617);
#5343=AXIS2_PLACEMENT_3D('',#19707,#6618,#6619);
#5344=AXIS2_PLACEMENT_3D('',#19709,#6621,#6622);
#5345=AXIS2_PLACEMENT_3D('',#19711,#6623,#6624);
#5346=AXIS2_PLACEMENT_3D('',#19713,#6626,#6627);
#5347=AXIS2_PLACEMENT_3D('',#19715,#6628,#6629);
#5348=AXIS2_PLACEMENT_3D('',#19717,#6631,#6632);
#5349=AXIS2_PLACEMENT_3D('',#19721,#6635,#6636);
#5350=AXIS2_PLACEMENT_3D('',#19722,#6637,#6638);
#5351=AXIS2_PLACEMENT_3D('',#19723,#6639,#6640);
#5352=AXIS2_PLACEMENT_3D('',#19724,#6641,#6642);
#5353=AXIS2_PLACEMENT_3D('',#19725,#6643,#6644);
#5354=AXIS2_PLACEMENT_3D('',#19727,#6645,#6646);
#5355=AXIS2_PLACEMENT_3D('',#19730,#6648,#6649);
#5356=AXIS2_PLACEMENT_3D('',#19731,#6650,#6651);
#5357=AXIS2_PLACEMENT_3D('',#19733,#6652,#6653);
#5358=AXIS2_PLACEMENT_3D('',#19736,#6655,#6656);
#5359=AXIS2_PLACEMENT_3D('',#19737,#6657,#6658);
#5360=AXIS2_PLACEMENT_3D('',#19740,#6659,#6660);
#5361=AXIS2_PLACEMENT_3D('',#19744,#6662,#6663);
#5362=AXIS2_PLACEMENT_3D('',#19746,#6665,#6666);
#5363=AXIS2_PLACEMENT_3D('',#19749,#6667,#6668);
#5364=AXIS2_PLACEMENT_3D('',#19751,#6669,#6670);
#5365=AXIS2_PLACEMENT_3D('',#19752,#6671,#6672);
#5366=AXIS2_PLACEMENT_3D('',#19753,#6673,#6674);
#5367=AXIS2_PLACEMENT_3D('',#19754,#6675,#6676);
#5368=AXIS2_PLACEMENT_3D('',#19755,#6677,#6678);
#5369=AXIS2_PLACEMENT_3D('',#19756,#6679,#6680);
#5370=AXIS2_PLACEMENT_3D('',#19758,#6681,#6682);
#5371=AXIS2_PLACEMENT_3D('',#19762,#6684,#6685);
#5372=AXIS2_PLACEMENT_3D('',#19764,#6687,#6688);
#5373=AXIS2_PLACEMENT_3D('',#19765,#6689,#6690);
#5374=AXIS2_PLACEMENT_3D('',#19766,#6691,#6692);
#5375=AXIS2_PLACEMENT_3D('',#19773,#6697,#6698);
#5376=AXIS2_PLACEMENT_3D('',#19776,#6700,#6701);
#5377=AXIS2_PLACEMENT_3D('',#19777,#6702,#6703);
#5378=AXIS2_PLACEMENT_3D('',#19781,#6705,#6706);
#5379=AXIS2_PLACEMENT_3D('',#19784,#6708,#6709);
#5380=AXIS2_PLACEMENT_3D('',#19786,#6710,#6711);
#5381=AXIS2_PLACEMENT_3D('',#19787,#6712,#6713);
#5382=AXIS2_PLACEMENT_3D('',#19790,#6715,#6716);
#5383=AXIS2_PLACEMENT_3D('',#19791,#6717,#6718);
#5384=AXIS2_PLACEMENT_3D('',#19796,#6722,#6723);
#5385=AXIS2_PLACEMENT_3D('',#19798,#6724,#6725);
#5386=AXIS2_PLACEMENT_3D('',#19799,#6726,#6727);
#5387=AXIS2_PLACEMENT_3D('',#19800,#6728,#6729);
#5388=AXIS2_PLACEMENT_3D('',#19802,#6730,#6731);
#5389=AXIS2_PLACEMENT_3D('',#19804,#6733,#6734);
#5390=AXIS2_PLACEMENT_3D('',#19805,#6735,#6736);
#5391=AXIS2_PLACEMENT_3D('',#19806,#6737,#6738);
#5392=AXIS2_PLACEMENT_3D('',#19808,#6739,#6740);
#5393=AXIS2_PLACEMENT_3D('',#19810,#6742,#6743);
#5394=AXIS2_PLACEMENT_3D('',#19813,#6745,#6746);
#5395=AXIS2_PLACEMENT_3D('',#19814,#6747,#6748);
#5396=AXIS2_PLACEMENT_3D('',#19817,#6750,#6751);
#5397=AXIS2_PLACEMENT_3D('',#19818,#6752,#6753);
#5398=AXIS2_PLACEMENT_3D('',#19822,#6756,#6757);
#5399=AXIS2_PLACEMENT_3D('',#19823,#6758,#6759);
#5400=AXIS2_PLACEMENT_3D('',#19824,#6760,#6761);
#5401=AXIS2_PLACEMENT_3D('',#19825,#6762,#6763);
#5402=AXIS2_PLACEMENT_3D('',#19826,#6764,#6765);
#5403=AXIS2_PLACEMENT_3D('',#19828,#6766,#6767);
#5404=AXIS2_PLACEMENT_3D('',#19831,#6769,#6770);
#5405=AXIS2_PLACEMENT_3D('',#19832,#6771,#6772);
#5406=AXIS2_PLACEMENT_3D('',#19833,#6773,#6774);
#5407=AXIS2_PLACEMENT_3D('',#19834,#6775,#6776);
#5408=AXIS2_PLACEMENT_3D('',#19836,#6777,#6778);
#5409=AXIS2_PLACEMENT_3D('',#19837,#6779,#6780);
#5410=AXIS2_PLACEMENT_3D('',#19839,#6781,#6782);
#5411=AXIS2_PLACEMENT_3D('',#19841,#6784,#6785);
#5412=AXIS2_PLACEMENT_3D('',#19843,#6786,#6787);
#5413=AXIS2_PLACEMENT_3D('',#19844,#6788,#6789);
#5414=AXIS2_PLACEMENT_3D('',#19846,#6790,#6791);
#5415=AXIS2_PLACEMENT_3D('',#19848,#6793,#6794);
#5416=AXIS2_PLACEMENT_3D('',#19849,#6795,#6796);
#5417=AXIS2_PLACEMENT_3D('',#19850,#6797,#6798);
#5418=AXIS2_PLACEMENT_3D('',#19852,#6799,#6800);
#5419=AXIS2_PLACEMENT_3D('',#19853,#6801,#6802);
#5420=AXIS2_PLACEMENT_3D('',#19854,#6803,#6804);
#5421=AXIS2_PLACEMENT_3D('',#19855,#6805,#6806);
#5422=AXIS2_PLACEMENT_3D('',#19856,#6807,#6808);
#5423=AXIS2_PLACEMENT_3D('',#19857,#6809,#6810);
#5424=AXIS2_PLACEMENT_3D('',#19858,#6811,#6812);
#5425=AXIS2_PLACEMENT_3D('',#19859,#6813,#6814);
#5426=AXIS2_PLACEMENT_3D('',#19860,#6815,#6816);
#5427=DIRECTION('axis',(0.,0.,1.));
#5428=DIRECTION('refdir',(1.,0.,0.));
#5429=DIRECTION('axis',(0.,0.,1.));
#5430=DIRECTION('refdir',(1.,0.,0.));
#5431=DIRECTION('center_axis',(0.,0.,-1.));
#5432=DIRECTION('ref_axis',(-1.,0.,0.));
#5433=DIRECTION('center_axis',(0.,0.,-1.));
#5434=DIRECTION('ref_axis',(-1.,0.,0.));
#5435=DIRECTION('',(0.,0.,-1.));
#5436=DIRECTION('center_axis',(0.,0.,1.));
#5437=DIRECTION('ref_axis',(-1.,0.,0.));
#5438=DIRECTION('center_axis',(0.,0.,-1.));
#5439=DIRECTION('ref_axis',(-0.830130914723544,-0.557568528900486,0.));
#5440=DIRECTION('center_axis',(0.,0.,-1.));
#5441=DIRECTION('ref_axis',(-0.830130914723544,-0.557568528900486,0.));
#5442=DIRECTION('',(0.,0.,-1.));
#5443=DIRECTION('center_axis',(0.,0.,-1.));
#5444=DIRECTION('ref_axis',(-0.830130914723544,-0.557568528900486,0.));
#5445=DIRECTION('',(0.,0.,1.));
#5446=DIRECTION('center_axis',(0.21892739748686,0.975741151448288,0.));
#5447=DIRECTION('ref_axis',(-0.975741151448288,0.21892739748686,0.));
#5448=DIRECTION('',(-0.975741151448288,0.21892739748686,0.));
#5449=DIRECTION('',(0.,0.,1.));
#5450=DIRECTION('',(0.975741151448288,-0.21892739748686,0.));
#5451=DIRECTION('center_axis',(0.,0.,1.));
#5452=DIRECTION('ref_axis',(-0.343859459137252,0.939021124555692,0.));
#5453=DIRECTION('center_axis',(0.,0.,-1.));
#5454=DIRECTION('ref_axis',(-0.343859459137252,0.939021124555692,0.));
#5455=DIRECTION('',(0.,0.,1.));
#5456=DIRECTION('center_axis',(0.,0.,-1.));
#5457=DIRECTION('ref_axis',(-0.343859459137252,0.939021124555692,0.));
#5458=DIRECTION('',(0.,0.,-1.));
#5459=DIRECTION('center_axis',(-0.396410273775032,-0.918073469198192,0.));
#5460=DIRECTION('ref_axis',(0.918073469198192,-0.396410273775032,0.));
#5461=DIRECTION('',(0.918073469198192,-0.396410273775032,0.));
#5462=DIRECTION('',(0.,0.,1.));
#5463=DIRECTION('',(0.918073469198192,-0.396410273775032,0.));
#5464=DIRECTION('center_axis',(0.,0.,-1.));
#5465=DIRECTION('ref_axis',(-0.961799566784773,-0.273754622486313,0.));
#5466=DIRECTION('center_axis',(0.,0.,-1.));
#5467=DIRECTION('ref_axis',(-0.961799566784773,-0.273754622486313,0.));
#5468=DIRECTION('',(0.,0.,-1.));
#5469=DIRECTION('center_axis',(0.,0.,-1.));
#5470=DIRECTION('ref_axis',(-0.961799566784773,-0.273754622486313,0.));
#5471=DIRECTION('',(0.,0.,1.));
#5472=DIRECTION('center_axis',(0.509732925883917,0.860332693944512,0.));
#5473=DIRECTION('ref_axis',(-0.860332693944512,0.509732925883917,0.));
#5474=DIRECTION('',(-0.860332693944512,0.509732925883917,0.));
#5475=DIRECTION('',(0.,0.,1.));
#5476=DIRECTION('',(0.860332693944512,-0.509732925883917,0.));
#5477=DIRECTION('center_axis',(0.,0.,1.));
#5478=DIRECTION('ref_axis',(-0.0368562937374252,0.999320575997483,0.));
#5479=DIRECTION('center_axis',(0.,0.,-1.));
#5480=DIRECTION('ref_axis',(-0.0368562937374252,0.999320575997483,0.));
#5481=DIRECTION('',(0.,0.,1.));
#5482=DIRECTION('center_axis',(0.,0.,-1.));
#5483=DIRECTION('ref_axis',(-0.0368562937374252,0.999320575997483,0.));
#5484=DIRECTION('',(0.,0.,-1.));
#5485=DIRECTION('center_axis',(-0.660708878067096,-0.750642243977328,0.));
#5486=DIRECTION('ref_axis',(0.750642243977328,-0.660708878067096,0.));
#5487=DIRECTION('',(0.750642243977328,-0.660708878067096,0.));
#5488=DIRECTION('',(0.,0.,1.));
#5489=DIRECTION('',(0.750642243977328,-0.660708878067096,0.));
#5490=DIRECTION('center_axis',(0.,0.,-1.));
#5491=DIRECTION('ref_axis',(-0.999320575997483,0.0368562937374283,0.));
#5492=DIRECTION('center_axis',(0.,0.,-1.));
#5493=DIRECTION('ref_axis',(-0.999320575997483,0.0368562937374283,0.));
#5494=DIRECTION('',(0.,0.,-1.));
#5495=DIRECTION('center_axis',(0.,0.,-1.));
#5496=DIRECTION('ref_axis',(-0.999320575997483,0.0368562937374283,0.));
#5497=DIRECTION('',(0.,0.,1.));
#5498=DIRECTION('center_axis',(0.750642243977329,0.660708878067096,0.));
#5499=DIRECTION('ref_axis',(-0.660708878067096,0.750642243977329,0.));
#5500=DIRECTION('',(-0.660708878067096,0.750642243977329,0.));
#5501=DIRECTION('',(0.,0.,1.));
#5502=DIRECTION('',(0.660708878067096,-0.750642243977329,0.));
#5503=DIRECTION('center_axis',(0.,0.,1.));
#5504=DIRECTION('ref_axis',(0.273754622486313,0.961799566784773,0.));
#5505=DIRECTION('center_axis',(0.,0.,-1.));
#5506=DIRECTION('ref_axis',(0.273754622486313,0.961799566784773,0.));
#5507=DIRECTION('',(0.,0.,1.));
#5508=DIRECTION('center_axis',(0.,0.,-1.));
#5509=DIRECTION('ref_axis',(0.273754622486313,0.961799566784773,0.));
#5510=DIRECTION('',(0.,0.,-1.));
#5511=DIRECTION('center_axis',(-0.860332693944512,-0.509732925883917,0.));
#5512=DIRECTION('ref_axis',(0.509732925883917,-0.860332693944512,0.));
#5513=DIRECTION('',(0.509732925883917,-0.860332693944512,0.));
#5514=DIRECTION('',(0.,0.,1.));
#5515=DIRECTION('',(0.509732925883917,-0.860332693944512,0.));
#5516=DIRECTION('center_axis',(0.,0.,-1.));
#5517=DIRECTION('ref_axis',(-0.939021124555692,0.343859459137252,0.));
#5518=DIRECTION('center_axis',(0.,0.,-1.));
#5519=DIRECTION('ref_axis',(-0.939021124555692,0.343859459137252,0.));
#5520=DIRECTION('',(0.,0.,-1.));
#5521=DIRECTION('center_axis',(0.,0.,-1.));
#5522=DIRECTION('ref_axis',(-0.939021124555692,0.343859459137252,0.));
#5523=DIRECTION('',(0.,0.,1.));
#5524=DIRECTION('center_axis',(0.918073469198192,0.396410273775032,0.));
#5525=DIRECTION('ref_axis',(-0.396410273775032,0.918073469198192,0.));
#5526=DIRECTION('',(-0.396410273775032,0.918073469198192,0.));
#5527=DIRECTION('',(0.,0.,1.));
#5528=DIRECTION('',(0.396410273775032,-0.918073469198192,0.));
#5529=DIRECTION('center_axis',(0.,0.,1.));
#5530=DIRECTION('ref_axis',(0.557568528900487,0.830130914723543,0.));
#5531=DIRECTION('center_axis',(0.,0.,-1.));
#5532=DIRECTION('ref_axis',(0.557568528900487,0.830130914723543,0.));
#5533=DIRECTION('',(0.,0.,1.));
#5534=DIRECTION('center_axis',(0.,0.,-1.));
#5535=DIRECTION('ref_axis',(0.557568528900487,0.830130914723543,0.));
#5536=DIRECTION('',(0.,0.,-1.));
#5537=DIRECTION('center_axis',(-0.975741151448288,-0.218927397486859,0.));
#5538=DIRECTION('ref_axis',(0.218927397486859,-0.975741151448288,0.));
#5539=DIRECTION('',(0.218927397486859,-0.975741151448288,0.));
#5540=DIRECTION('',(0.,0.,1.));
#5541=DIRECTION('',(0.218927397486859,-0.975741151448288,0.));
#5542=DIRECTION('center_axis',(0.,0.,-1.));
#5543=DIRECTION('ref_axis',(-0.786803742897506,0.617203264866993,0.));
#5544=DIRECTION('center_axis',(0.,0.,-1.));
#5545=DIRECTION('ref_axis',(-0.786803742897506,0.617203264866993,0.));
#5546=DIRECTION('',(0.,0.,-1.));
#5547=DIRECTION('center_axis',(0.,0.,-1.));
#5548=DIRECTION('ref_axis',(-0.786803742897506,0.617203264866993,0.));
#5549=DIRECTION('',(0.,0.,1.));
#5550=DIRECTION('center_axis',(0.995637266659949,0.0933082699330834,0.));
#5551=DIRECTION('ref_axis',(-0.0933082699330834,0.995637266659949,0.));
#5552=DIRECTION('',(-0.0933082699330834,0.995637266659949,0.));
#5553=DIRECTION('',(0.,0.,1.));
#5554=DIRECTION('',(0.0933082699330834,-0.995637266659949,0.));
#5555=DIRECTION('center_axis',(0.,0.,1.));
#5556=DIRECTION('ref_axis',(0.786803742897505,0.617203264866994,0.));
#5557=DIRECTION('center_axis',(0.,0.,-1.));
#5558=DIRECTION('ref_axis',(0.786803742897505,0.617203264866994,0.));
#5559=DIRECTION('',(0.,0.,1.));
#5560=DIRECTION('center_axis',(0.,0.,-1.));
#5561=DIRECTION('ref_axis',(0.786803742897505,0.617203264866994,0.));
#5562=DIRECTION('',(0.,0.,-1.));
#5563=DIRECTION('center_axis',(-0.995637266659949,0.0933082699330838,0.));
#5564=DIRECTION('ref_axis',(-0.0933082699330838,-0.995637266659949,0.));
#5565=DIRECTION('',(-0.0933082699330838,-0.995637266659949,0.));
#5566=DIRECTION('',(0.,0.,1.));
#5567=DIRECTION('',(-0.0933082699330838,-0.995637266659949,0.));
#5568=DIRECTION('center_axis',(0.,0.,-1.));
#5569=DIRECTION('ref_axis',(-0.557568528900486,0.830130914723544,0.));
#5570=DIRECTION('center_axis',(0.,0.,-1.));
#5571=DIRECTION('ref_axis',(-0.557568528900486,0.830130914723544,0.));
#5572=DIRECTION('',(0.,0.,-1.));
#5573=DIRECTION('center_axis',(0.,0.,-1.));
#5574=DIRECTION('ref_axis',(-0.557568528900486,0.830130914723544,0.));
#5575=DIRECTION('',(0.,0.,1.));
#5576=DIRECTION('center_axis',(0.975741151448288,-0.21892739748686,0.));
#5577=DIRECTION('ref_axis',(0.21892739748686,0.975741151448288,0.));
#5578=DIRECTION('',(0.21892739748686,0.975741151448288,0.));
#5579=DIRECTION('',(0.,0.,1.));
#5580=DIRECTION('',(-0.21892739748686,-0.975741151448288,0.));
#5581=DIRECTION('center_axis',(0.,0.,1.));
#5582=DIRECTION('ref_axis',(0.939021124555691,0.343859459137256,0.));
#5583=DIRECTION('center_axis',(0.,0.,-1.));
#5584=DIRECTION('ref_axis',(0.939021124555691,0.343859459137256,0.));
#5585=DIRECTION('',(0.,0.,1.));
#5586=DIRECTION('center_axis',(0.,0.,-1.));
#5587=DIRECTION('ref_axis',(0.939021124555691,0.343859459137256,0.));
#5588=DIRECTION('',(0.,0.,-1.));
#5589=DIRECTION('center_axis',(-0.918073469198192,0.396410273775032,0.));
#5590=DIRECTION('ref_axis',(-0.396410273775032,-0.918073469198192,0.));
#5591=DIRECTION('',(-0.396410273775032,-0.918073469198192,0.));
#5592=DIRECTION('',(0.,0.,1.));
#5593=DIRECTION('',(-0.396410273775032,-0.918073469198192,0.));
#5594=DIRECTION('center_axis',(0.,0.,-1.));
#5595=DIRECTION('ref_axis',(-0.273754622486312,0.961799566784773,0.));
#5596=DIRECTION('center_axis',(0.,0.,-1.));
#5597=DIRECTION('ref_axis',(-0.273754622486312,0.961799566784773,0.));
#5598=DIRECTION('',(0.,0.,-1.));
#5599=DIRECTION('center_axis',(0.,0.,-1.));
#5600=DIRECTION('ref_axis',(-0.273754622486312,0.961799566784773,0.));
#5601=DIRECTION('',(0.,0.,1.));
#5602=DIRECTION('center_axis',(0.860332693944512,-0.509732925883917,0.));
#5603=DIRECTION('ref_axis',(0.509732925883917,0.860332693944512,0.));
#5604=DIRECTION('',(0.509732925883917,0.860332693944512,0.));
#5605=DIRECTION('',(0.,0.,1.));
#5606=DIRECTION('',(-0.509732925883917,-0.860332693944512,0.));
#5607=DIRECTION('center_axis',(0.,0.,1.));
#5608=DIRECTION('ref_axis',(0.999320575997482,0.0368562937374314,0.));
#5609=DIRECTION('center_axis',(0.,0.,-1.));
#5610=DIRECTION('ref_axis',(0.999320575997482,0.0368562937374314,0.));
#5611=DIRECTION('',(0.,0.,1.));
#5612=DIRECTION('center_axis',(0.,0.,-1.));
#5613=DIRECTION('ref_axis',(0.999320575997482,0.0368562937374314,0.));
#5614=DIRECTION('',(0.,0.,-1.));
#5615=DIRECTION('center_axis',(-0.750642243977328,0.660708878067096,0.));
#5616=DIRECTION('ref_axis',(-0.660708878067096,-0.750642243977328,0.));
#5617=DIRECTION('',(-0.660708878067096,-0.750642243977328,0.));
#5618=DIRECTION('',(0.,0.,1.));
#5619=DIRECTION('',(-0.660708878067096,-0.750642243977328,0.));
#5620=DIRECTION('center_axis',(0.,0.,-1.));
#5621=DIRECTION('ref_axis',(0.0368562937374315,0.999320575997482,0.));
#5622=DIRECTION('center_axis',(0.,0.,-1.));
#5623=DIRECTION('ref_axis',(0.0368562937374315,0.999320575997482,0.));
#5624=DIRECTION('',(0.,0.,-1.));
#5625=DIRECTION('center_axis',(0.,0.,-1.));
#5626=DIRECTION('ref_axis',(0.0368562937374315,0.999320575997482,0.));
#5627=DIRECTION('',(0.,0.,1.));
#5628=DIRECTION('center_axis',(0.660708878067096,-0.750642243977329,0.));
#5629=DIRECTION('ref_axis',(0.750642243977329,0.660708878067096,0.));
#5630=DIRECTION('',(0.750642243977329,0.660708878067096,0.));
#5631=DIRECTION('',(0.,0.,1.));
#5632=DIRECTION('',(-0.750642243977328,-0.660708878067096,0.));
#5633=DIRECTION('center_axis',(0.,0.,1.));
#5634=DIRECTION('ref_axis',(0.961799566784773,-0.273754622486311,0.));
#5635=DIRECTION('center_axis',(0.,0.,-1.));
#5636=DIRECTION('ref_axis',(0.961799566784773,-0.273754622486311,0.));
#5637=DIRECTION('',(0.,0.,1.));
#5638=DIRECTION('center_axis',(0.,0.,-1.));
#5639=DIRECTION('ref_axis',(0.961799566784773,-0.273754622486311,0.));
#5640=DIRECTION('',(0.,0.,-1.));
#5641=DIRECTION('center_axis',(-0.509732925883917,0.860332693944512,0.));
#5642=DIRECTION('ref_axis',(-0.860332693944512,-0.509732925883917,0.));
#5643=DIRECTION('',(-0.860332693944512,-0.509732925883917,0.));
#5644=DIRECTION('',(0.,0.,1.));
#5645=DIRECTION('',(-0.860332693944512,-0.509732925883917,0.));
#5646=DIRECTION('center_axis',(0.,0.,-1.));
#5647=DIRECTION('ref_axis',(0.343859459137253,0.939021124555692,0.));
#5648=DIRECTION('center_axis',(0.,0.,-1.));
#5649=DIRECTION('ref_axis',(0.343859459137253,0.939021124555692,0.));
#5650=DIRECTION('',(0.,0.,-1.));
#5651=DIRECTION('center_axis',(0.,0.,-1.));
#5652=DIRECTION('ref_axis',(0.343859459137253,0.939021124555692,0.));
#5653=DIRECTION('',(0.,0.,1.));
#5654=DIRECTION('center_axis',(0.396410273775032,-0.918073469198192,0.));
#5655=DIRECTION('ref_axis',(0.918073469198192,0.396410273775032,0.));
#5656=DIRECTION('',(0.918073469198192,0.396410273775032,0.));
#5657=DIRECTION('',(0.,0.,1.));
#5658=DIRECTION('',(-0.918073469198192,-0.396410273775032,0.));
#5659=DIRECTION('center_axis',(0.,0.,1.));
#5660=DIRECTION('ref_axis',(0.830130914723543,-0.557568528900488,0.));
#5661=DIRECTION('center_axis',(0.,0.,-1.));
#5662=DIRECTION('ref_axis',(0.830130914723543,-0.557568528900488,0.));
#5663=DIRECTION('',(0.,0.,1.));
#5664=DIRECTION('center_axis',(0.,0.,-1.));
#5665=DIRECTION('ref_axis',(0.830130914723543,-0.557568528900488,0.));
#5666=DIRECTION('',(0.,0.,-1.));
#5667=DIRECTION('center_axis',(-0.218927397486859,0.975741151448288,0.));
#5668=DIRECTION('ref_axis',(-0.975741151448288,-0.218927397486859,0.));
#5669=DIRECTION('',(-0.975741151448288,-0.218927397486859,0.));
#5670=DIRECTION('',(0.,0.,1.));
#5671=DIRECTION('',(-0.975741151448288,-0.218927397486859,0.));
#5672=DIRECTION('center_axis',(0.,0.,-1.));
#5673=DIRECTION('ref_axis',(0.617203264866995,0.786803742897504,0.));
#5674=DIRECTION('center_axis',(0.,0.,-1.));
#5675=DIRECTION('ref_axis',(0.617203264866995,0.786803742897504,0.));
#5676=DIRECTION('',(0.,0.,-1.));
#5677=DIRECTION('center_axis',(0.,0.,-1.));
#5678=DIRECTION('ref_axis',(0.617203264866995,0.786803742897504,0.));
#5679=DIRECTION('',(0.,0.,1.));
#5680=DIRECTION('center_axis',(0.0933082699330836,-0.995637266659949,0.));
#5681=DIRECTION('ref_axis',(0.995637266659949,0.0933082699330836,0.));
#5682=DIRECTION('',(0.995637266659949,0.0933082699330836,0.));
#5683=DIRECTION('',(0.,0.,1.));
#5684=DIRECTION('',(-0.995637266659949,-0.0933082699330836,0.));
#5685=DIRECTION('center_axis',(0.,0.,1.));
#5686=DIRECTION('ref_axis',(0.617203264866993,-0.786803742897506,0.));
#5687=DIRECTION('center_axis',(0.,0.,-1.));
#5688=DIRECTION('ref_axis',(0.617203264866993,-0.786803742897506,0.));
#5689=DIRECTION('',(0.,0.,1.));
#5690=DIRECTION('center_axis',(0.,0.,-1.));
#5691=DIRECTION('ref_axis',(0.617203264866993,-0.786803742897506,0.));
#5692=DIRECTION('',(0.,0.,-1.));
#5693=DIRECTION('center_axis',(0.0933082699330837,0.995637266659949,0.));
#5694=DIRECTION('ref_axis',(-0.995637266659949,0.0933082699330837,0.));
#5695=DIRECTION('',(-0.995637266659949,0.0933082699330837,0.));
#5696=DIRECTION('',(0.,0.,1.));
#5697=DIRECTION('',(-0.995637266659949,0.0933082699330837,0.));
#5698=DIRECTION('center_axis',(0.,0.,-1.));
#5699=DIRECTION('ref_axis',(0.830130914723545,0.557568528900485,0.));
#5700=DIRECTION('center_axis',(0.,0.,-1.));
#5701=DIRECTION('ref_axis',(0.830130914723545,0.557568528900485,0.));
#5702=DIRECTION('',(0.,0.,-1.));
#5703=DIRECTION('center_axis',(0.,0.,-1.));
#5704=DIRECTION('ref_axis',(0.830130914723545,0.557568528900485,0.));
#5705=DIRECTION('',(0.,0.,1.));
#5706=DIRECTION('center_axis',(-0.218927397486859,-0.975741151448288,0.));
#5707=DIRECTION('ref_axis',(0.975741151448288,-0.218927397486859,0.));
#5708=DIRECTION('',(0.975741151448288,-0.218927397486859,0.));
#5709=DIRECTION('',(0.,0.,1.));
#5710=DIRECTION('',(-0.975741151448288,0.218927397486859,0.));
#5711=DIRECTION('center_axis',(0.,0.,1.));
#5712=DIRECTION('ref_axis',(0.343859459137252,-0.939021124555692,0.));
#5713=DIRECTION('center_axis',(0.,0.,-1.));
#5714=DIRECTION('ref_axis',(0.343859459137252,-0.939021124555692,0.));
#5715=DIRECTION('',(0.,0.,1.));
#5716=DIRECTION('center_axis',(0.,0.,-1.));
#5717=DIRECTION('ref_axis',(0.343859459137252,-0.939021124555692,0.));
#5718=DIRECTION('',(0.,0.,-1.));
#5719=DIRECTION('center_axis',(0.396410273775032,0.918073469198192,0.));
#5720=DIRECTION('ref_axis',(-0.918073469198192,0.396410273775032,0.));
#5721=DIRECTION('',(-0.918073469198192,0.396410273775032,0.));
#5722=DIRECTION('',(0.,0.,1.));
#5723=DIRECTION('',(-0.918073469198192,0.396410273775032,0.));
#5724=DIRECTION('center_axis',(0.,0.,-1.));
#5725=DIRECTION('ref_axis',(0.961799566784772,0.273754622486314,0.));
#5726=DIRECTION('center_axis',(0.,0.,-1.));
#5727=DIRECTION('ref_axis',(0.961799566784772,0.273754622486314,0.));
#5728=DIRECTION('',(0.,0.,-1.));
#5729=DIRECTION('center_axis',(0.,0.,-1.));
#5730=DIRECTION('ref_axis',(0.961799566784772,0.273754622486314,0.));
#5731=DIRECTION('',(0.,0.,1.));
#5732=DIRECTION('center_axis',(-0.509732925883917,-0.860332693944512,0.));
#5733=DIRECTION('ref_axis',(0.860332693944512,-0.509732925883917,0.));
#5734=DIRECTION('',(0.860332693944512,-0.509732925883917,0.));
#5735=DIRECTION('',(0.,0.,1.));
#5736=DIRECTION('',(-0.860332693944512,0.509732925883917,0.));
#5737=DIRECTION('center_axis',(0.,0.,1.));
#5738=DIRECTION('ref_axis',(0.0368562937374283,-0.999320575997483,0.));
#5739=DIRECTION('center_axis',(0.,0.,-1.));
#5740=DIRECTION('ref_axis',(0.0368562937374283,-0.999320575997483,0.));
#5741=DIRECTION('',(0.,0.,1.));
#5742=DIRECTION('center_axis',(0.,0.,-1.));
#5743=DIRECTION('ref_axis',(0.0368562937374283,-0.999320575997483,0.));
#5744=DIRECTION('',(0.,0.,-1.));
#5745=DIRECTION('center_axis',(0.660708878067096,0.750642243977328,0.));
#5746=DIRECTION('ref_axis',(-0.750642243977328,0.660708878067096,0.));
#5747=DIRECTION('',(-0.750642243977328,0.660708878067096,0.));
#5748=DIRECTION('',(0.,0.,1.));
#5749=DIRECTION('',(-0.750642243977328,0.660708878067096,0.));
#5750=DIRECTION('center_axis',(0.,0.,-1.));
#5751=DIRECTION('ref_axis',(0.999320575997483,-0.0368562937374252,0.));
#5752=DIRECTION('center_axis',(0.,0.,-1.));
#5753=DIRECTION('ref_axis',(0.999320575997483,-0.0368562937374252,0.));
#5754=DIRECTION('',(0.,0.,-1.));
#5755=DIRECTION('center_axis',(0.,0.,-1.));
#5756=DIRECTION('ref_axis',(0.999320575997483,-0.0368562937374252,0.));
#5757=DIRECTION('',(0.,0.,1.));
#5758=DIRECTION('center_axis',(-0.750642243977329,-0.660708878067096,0.));
#5759=DIRECTION('ref_axis',(0.660708878067096,-0.750642243977329,0.));
#5760=DIRECTION('',(0.660708878067096,-0.750642243977329,0.));
#5761=DIRECTION('',(0.,0.,1.));
#5762=DIRECTION('',(-0.660708878067096,0.750642243977328,0.));
#5763=DIRECTION('center_axis',(0.,0.,1.));
#5764=DIRECTION('ref_axis',(-0.273754622486316,-0.961799566784772,0.));
#5765=DIRECTION('center_axis',(0.,0.,-1.));
#5766=DIRECTION('ref_axis',(-0.273754622486316,-0.961799566784772,0.));
#5767=DIRECTION('',(0.,0.,1.));
#5768=DIRECTION('center_axis',(0.,0.,-1.));
#5769=DIRECTION('ref_axis',(-0.273754622486316,-0.961799566784772,0.));
#5770=DIRECTION('',(0.,0.,-1.));
#5771=DIRECTION('center_axis',(0.860332693944512,0.509732925883917,0.));
#5772=DIRECTION('ref_axis',(-0.509732925883917,0.860332693944512,0.));
#5773=DIRECTION('',(-0.509732925883917,0.860332693944512,0.));
#5774=DIRECTION('',(0.,0.,1.));
#5775=DIRECTION('',(-0.509732925883917,0.860332693944512,0.));
#5776=DIRECTION('center_axis',(0.,0.,-1.));
#5777=DIRECTION('ref_axis',(0.939021124555692,-0.343859459137252,0.));
#5778=DIRECTION('center_axis',(0.,0.,-1.));
#5779=DIRECTION('ref_axis',(0.939021124555692,-0.343859459137252,0.));
#5780=DIRECTION('',(0.,0.,-1.));
#5781=DIRECTION('center_axis',(0.,0.,-1.));
#5782=DIRECTION('ref_axis',(0.939021124555692,-0.343859459137252,0.));
#5783=DIRECTION('',(0.,0.,1.));
#5784=DIRECTION('center_axis',(-0.918073469198192,-0.396410273775032,0.));
#5785=DIRECTION('ref_axis',(0.396410273775032,-0.918073469198192,0.));
#5786=DIRECTION('',(0.396410273775032,-0.918073469198192,0.));
#5787=DIRECTION('',(0.,0.,1.));
#5788=DIRECTION('',(-0.396410273775032,0.918073469198192,0.));
#5789=DIRECTION('center_axis',(0.,0.,1.));
#5790=DIRECTION('ref_axis',(-0.557568528900488,-0.830130914723543,0.));
#5791=DIRECTION('center_axis',(0.,0.,-1.));
#5792=DIRECTION('ref_axis',(-0.557568528900488,-0.830130914723543,0.));
#5793=DIRECTION('',(0.,0.,1.));
#5794=DIRECTION('center_axis',(0.,0.,-1.));
#5795=DIRECTION('ref_axis',(-0.557568528900488,-0.830130914723543,0.));
#5796=DIRECTION('',(0.,0.,-1.));
#5797=DIRECTION('center_axis',(0.975741151448288,0.218927397486859,0.));
#5798=DIRECTION('ref_axis',(-0.218927397486859,0.975741151448288,0.));
#5799=DIRECTION('',(-0.218927397486859,0.975741151448288,0.));
#5800=DIRECTION('',(0.,0.,1.));
#5801=DIRECTION('',(-0.218927397486859,0.975741151448288,0.));
#5802=DIRECTION('center_axis',(0.,0.,-1.));
#5803=DIRECTION('ref_axis',(0.786803742897506,-0.617203264866993,0.));
#5804=DIRECTION('center_axis',(0.,0.,-1.));
#5805=DIRECTION('ref_axis',(0.786803742897506,-0.617203264866993,0.));
#5806=DIRECTION('',(0.,0.,-1.));
#5807=DIRECTION('center_axis',(0.,0.,-1.));
#5808=DIRECTION('ref_axis',(0.786803742897506,-0.617203264866993,0.));
#5809=DIRECTION('',(0.,0.,1.));
#5810=DIRECTION('center_axis',(-0.995637266659949,-0.0933082699330836,0.));
#5811=DIRECTION('ref_axis',(0.0933082699330836,-0.995637266659949,0.));
#5812=DIRECTION('',(0.0933082699330836,-0.995637266659949,0.));
#5813=DIRECTION('',(0.,0.,1.));
#5814=DIRECTION('',(-0.0933082699330836,0.995637266659949,0.));
#5815=DIRECTION('center_axis',(0.,0.,1.));
#5816=DIRECTION('ref_axis',(-0.786803742897506,-0.617203264866993,0.));
#5817=DIRECTION('center_axis',(0.,0.,-1.));
#5818=DIRECTION('ref_axis',(-0.786803742897506,-0.617203264866993,0.));
#5819=DIRECTION('',(0.,0.,1.));
#5820=DIRECTION('center_axis',(0.,0.,-1.));
#5821=DIRECTION('ref_axis',(-0.786803742897506,-0.617203264866993,0.));
#5822=DIRECTION('',(0.,0.,-1.));
#5823=DIRECTION('center_axis',(0.995637266659949,-0.0933082699330837,0.));
#5824=DIRECTION('ref_axis',(0.0933082699330837,0.995637266659949,0.));
#5825=DIRECTION('',(0.0933082699330837,0.995637266659949,0.));
#5826=DIRECTION('',(0.,0.,1.));
#5827=DIRECTION('',(0.0933082699330837,0.995637266659949,0.));
#5828=DIRECTION('center_axis',(0.,0.,-1.));
#5829=DIRECTION('ref_axis',(0.557568528900485,-0.830130914723545,0.));
#5830=DIRECTION('center_axis',(0.,0.,-1.));
#5831=DIRECTION('ref_axis',(0.557568528900485,-0.830130914723545,0.));
#5832=DIRECTION('',(0.,0.,-1.));
#5833=DIRECTION('center_axis',(0.,0.,-1.));
#5834=DIRECTION('ref_axis',(0.557568528900485,-0.830130914723545,0.));
#5835=DIRECTION('',(0.,0.,1.));
#5836=DIRECTION('center_axis',(-0.975741151448288,0.218927397486859,0.));
#5837=DIRECTION('ref_axis',(-0.218927397486859,-0.975741151448288,0.));
#5838=DIRECTION('',(-0.218927397486859,-0.975741151448288,0.));
#5839=DIRECTION('',(0.,0.,1.));
#5840=DIRECTION('',(0.218927397486859,0.975741151448288,0.));
#5841=DIRECTION('center_axis',(0.,0.,1.));
#5842=DIRECTION('ref_axis',(-0.939021124555691,-0.343859459137255,0.));
#5843=DIRECTION('center_axis',(0.,0.,-1.));
#5844=DIRECTION('ref_axis',(-0.939021124555691,-0.343859459137255,0.));
#5845=DIRECTION('',(0.,0.,1.));
#5846=DIRECTION('center_axis',(0.,0.,-1.));
#5847=DIRECTION('ref_axis',(-0.939021124555691,-0.343859459137255,0.));
#5848=DIRECTION('',(0.,0.,-1.));
#5849=DIRECTION('center_axis',(0.918073469198192,-0.396410273775032,0.));
#5850=DIRECTION('ref_axis',(0.396410273775032,0.918073469198192,0.));
#5851=DIRECTION('',(0.396410273775032,0.918073469198192,0.));
#5852=DIRECTION('',(0.,0.,1.));
#5853=DIRECTION('',(0.396410273775032,0.918073469198192,0.));
#5854=DIRECTION('center_axis',(0.,0.,-1.));
#5855=DIRECTION('ref_axis',(0.273754622486314,-0.961799566784772,0.));
#5856=DIRECTION('center_axis',(0.,0.,-1.));
#5857=DIRECTION('ref_axis',(0.273754622486314,-0.961799566784772,0.));
#5858=DIRECTION('',(0.,0.,-1.));
#5859=DIRECTION('center_axis',(0.,0.,-1.));
#5860=DIRECTION('ref_axis',(0.273754622486314,-0.961799566784772,0.));
#5861=DIRECTION('',(0.,0.,1.));
#5862=DIRECTION('center_axis',(-0.860332693944512,0.509732925883917,0.));
#5863=DIRECTION('ref_axis',(-0.509732925883917,-0.860332693944512,0.));
#5864=DIRECTION('',(-0.509732925883917,-0.860332693944512,0.));
#5865=DIRECTION('',(0.,0.,1.));
#5866=DIRECTION('',(0.509732925883917,0.860332693944512,0.));
#5867=DIRECTION('center_axis',(0.,0.,1.));
#5868=DIRECTION('ref_axis',(-0.999320575997483,-0.0368562937374282,0.));
#5869=DIRECTION('center_axis',(0.,0.,-1.));
#5870=DIRECTION('ref_axis',(-0.999320575997483,-0.0368562937374282,0.));
#5871=DIRECTION('',(0.,0.,1.));
#5872=DIRECTION('center_axis',(0.,0.,-1.));
#5873=DIRECTION('ref_axis',(-0.999320575997483,-0.0368562937374282,0.));
#5874=DIRECTION('',(0.,0.,-1.));
#5875=DIRECTION('center_axis',(0.750642243977328,-0.660708878067096,0.));
#5876=DIRECTION('ref_axis',(0.660708878067096,0.750642243977328,0.));
#5877=DIRECTION('',(0.660708878067096,0.750642243977328,0.));
#5878=DIRECTION('',(0.,0.,1.));
#5879=DIRECTION('',(0.660708878067096,0.750642243977328,0.));
#5880=DIRECTION('center_axis',(0.,0.,-1.));
#5881=DIRECTION('ref_axis',(-0.0368562937374283,-0.999320575997483,0.));
#5882=DIRECTION('center_axis',(0.,0.,-1.));
#5883=DIRECTION('ref_axis',(-0.0368562937374283,-0.999320575997483,0.));
#5884=DIRECTION('',(0.,0.,-1.));
#5885=DIRECTION('center_axis',(0.,0.,-1.));
#5886=DIRECTION('ref_axis',(-0.0368562937374283,-0.999320575997483,0.));
#5887=DIRECTION('',(0.,0.,1.));
#5888=DIRECTION('center_axis',(-0.660708878067096,0.750642243977328,0.));
#5889=DIRECTION('ref_axis',(-0.750642243977328,-0.660708878067096,0.));
#5890=DIRECTION('',(-0.750642243977328,-0.660708878067096,0.));
#5891=DIRECTION('',(0.,0.,1.));
#5892=DIRECTION('',(0.750642243977328,0.660708878067096,0.));
#5893=DIRECTION('center_axis',(0.,0.,1.));
#5894=DIRECTION('ref_axis',(-0.961799566784773,0.273754622486313,0.));
#5895=DIRECTION('center_axis',(0.,0.,-1.));
#5896=DIRECTION('ref_axis',(-0.961799566784773,0.273754622486313,0.));
#5897=DIRECTION('',(0.,0.,1.));
#5898=DIRECTION('center_axis',(0.,0.,-1.));
#5899=DIRECTION('ref_axis',(-0.961799566784773,0.273754622486313,0.));
#5900=DIRECTION('',(0.,0.,-1.));
#5901=DIRECTION('center_axis',(0.509732925883917,-0.860332693944512,0.));
#5902=DIRECTION('ref_axis',(0.860332693944512,0.509732925883917,0.));
#5903=DIRECTION('',(0.860332693944512,0.509732925883917,0.));
#5904=DIRECTION('',(0.,0.,1.));
#5905=DIRECTION('',(0.860332693944512,0.509732925883917,0.));
#5906=DIRECTION('center_axis',(0.,0.,-1.));
#5907=DIRECTION('ref_axis',(-0.343859459137254,-0.939021124555691,0.));
#5908=DIRECTION('center_axis',(0.,0.,-1.));
#5909=DIRECTION('ref_axis',(-0.343859459137254,-0.939021124555691,0.));
#5910=DIRECTION('',(0.,0.,-1.));
#5911=DIRECTION('center_axis',(0.,0.,-1.));
#5912=DIRECTION('ref_axis',(-0.343859459137254,-0.939021124555691,0.));
#5913=DIRECTION('',(0.,0.,1.));
#5914=DIRECTION('center_axis',(-0.396410273775032,0.918073469198192,0.));
#5915=DIRECTION('ref_axis',(-0.918073469198192,-0.396410273775032,0.));
#5916=DIRECTION('',(-0.918073469198192,-0.396410273775032,0.));
#5917=DIRECTION('',(0.,0.,1.));
#5918=DIRECTION('',(0.918073469198192,0.396410273775032,0.));
#5919=DIRECTION('center_axis',(0.,0.,1.));
#5920=DIRECTION('ref_axis',(-0.830130914723544,0.557568528900486,0.));
#5921=DIRECTION('center_axis',(0.,0.,-1.));
#5922=DIRECTION('ref_axis',(-0.830130914723544,0.557568528900486,0.));
#5923=DIRECTION('',(0.,0.,1.));
#5924=DIRECTION('center_axis',(0.,0.,-1.));
#5925=DIRECTION('ref_axis',(-0.830130914723544,0.557568528900486,0.));
#5926=DIRECTION('',(0.,0.,-1.));
#5927=DIRECTION('center_axis',(0.218927397486859,-0.975741151448288,0.));
#5928=DIRECTION('ref_axis',(0.975741151448288,0.218927397486859,0.));
#5929=DIRECTION('',(0.975741151448288,0.218927397486859,0.));
#5930=DIRECTION('',(0.,0.,1.));
#5931=DIRECTION('',(0.975741151448288,0.218927397486859,0.));
#5932=DIRECTION('',(0.,0.,1.));
#5933=DIRECTION('center_axis',(0.,0.,1.));
#5934=DIRECTION('ref_axis',(0.940823330106451,-0.338897420361099,0.));
#5935=DIRECTION('center_axis',(0.,0.,1.));
#5936=DIRECTION('ref_axis',(0.940823330106451,-0.338897420361099,0.));
#5937=DIRECTION('center_axis',(0.,0.,1.));
#5938=DIRECTION('ref_axis',(0.940823330106451,-0.338897420361099,0.));
#5939=DIRECTION('',(0.,0.,1.));
#5940=DIRECTION('',(0.,0.,1.));
#5941=DIRECTION('center_axis',(0.,0.,1.));
#5942=DIRECTION('ref_axis',(0.790051096538837,-0.613040997697366,0.));
#5943=DIRECTION('center_axis',(0.,0.,1.));
#5944=DIRECTION('ref_axis',(0.790051096538837,-0.613040997697366,0.));
#5945=DIRECTION('center_axis',(0.,0.,1.));
#5946=DIRECTION('ref_axis',(0.790051096538837,-0.613040997697366,0.));
#5947=DIRECTION('',(0.,0.,1.));
#5948=DIRECTION('',(0.,0.,1.));
#5949=DIRECTION('center_axis',(0.,0.,1.));
#5950=DIRECTION('ref_axis',(0.561943157032333,-0.827175850871225,0.));
#5951=DIRECTION('center_axis',(0.,0.,1.));
#5952=DIRECTION('ref_axis',(0.561943157032333,-0.827175850871225,0.));
#5953=DIRECTION('center_axis',(0.,0.,1.));
#5954=DIRECTION('ref_axis',(0.561943157032333,-0.827175850871225,0.));
#5955=DIRECTION('',(0.,0.,1.));
#5956=DIRECTION('',(0.,0.,1.));
#5957=DIRECTION('center_axis',(0.,0.,1.));
#5958=DIRECTION('ref_axis',(0.278828306027306,-0.960340968488767,0.));
#5959=DIRECTION('center_axis',(0.,0.,1.));
#5960=DIRECTION('ref_axis',(0.278828306027306,-0.960340968488767,0.));
#5961=DIRECTION('center_axis',(0.,0.,1.));
#5962=DIRECTION('ref_axis',(0.278828306027306,-0.960340968488767,0.));
#5963=DIRECTION('',(0.,0.,1.));
#5964=DIRECTION('',(0.,0.,1.));
#5965=DIRECTION('center_axis',(0.,0.,1.));
#5966=DIRECTION('ref_axis',(-0.0315802022827165,-0.999501221021657,0.));
#5967=DIRECTION('center_axis',(0.,0.,1.));
#5968=DIRECTION('ref_axis',(-0.0315802022827165,-0.999501221021657,0.));
#5969=DIRECTION('center_axis',(0.,0.,1.));
#5970=DIRECTION('ref_axis',(-0.0315802022827165,-0.999501221021657,0.));
#5971=DIRECTION('',(0.,0.,1.));
#5972=DIRECTION('',(0.,0.,1.));
#5973=DIRECTION('center_axis',(0.,0.,1.));
#5974=DIRECTION('ref_axis',(-0.338897420361099,-0.940823330106451,0.));
#5975=DIRECTION('center_axis',(0.,0.,1.));
#5976=DIRECTION('ref_axis',(-0.338897420361099,-0.940823330106451,0.));
#5977=DIRECTION('center_axis',(0.,0.,1.));
#5978=DIRECTION('ref_axis',(-0.338897420361099,-0.940823330106451,0.));
#5979=DIRECTION('',(0.,0.,1.));
#5980=DIRECTION('',(0.,0.,1.));
#5981=DIRECTION('center_axis',(0.,0.,1.));
#5982=DIRECTION('ref_axis',(-0.613040997697366,-0.790051096538837,0.));
#5983=DIRECTION('center_axis',(0.,0.,1.));
#5984=DIRECTION('ref_axis',(-0.613040997697366,-0.790051096538837,0.));
#5985=DIRECTION('center_axis',(0.,0.,1.));
#5986=DIRECTION('ref_axis',(-0.613040997697366,-0.790051096538837,0.));
#5987=DIRECTION('',(0.,0.,1.));
#5988=DIRECTION('',(0.,0.,1.));
#5989=DIRECTION('center_axis',(0.,0.,1.));
#5990=DIRECTION('ref_axis',(-0.827175850871225,-0.561943157032333,0.));
#5991=DIRECTION('center_axis',(0.,0.,1.));
#5992=DIRECTION('ref_axis',(-0.827175850871225,-0.561943157032333,0.));
#5993=DIRECTION('center_axis',(0.,0.,1.));
#5994=DIRECTION('ref_axis',(-0.827175850871225,-0.561943157032333,0.));
#5995=DIRECTION('',(0.,0.,1.));
#5996=DIRECTION('',(0.,0.,1.));
#5997=DIRECTION('center_axis',(0.,0.,1.));
#5998=DIRECTION('ref_axis',(-0.960340968488767,-0.278828306027306,0.));
#5999=DIRECTION('center_axis',(0.,0.,1.));
#6000=DIRECTION('ref_axis',(-0.960340968488767,-0.278828306027306,0.));
#6001=DIRECTION('center_axis',(0.,0.,1.));
#6002=DIRECTION('ref_axis',(-0.960340968488767,-0.278828306027306,0.));
#6003=DIRECTION('',(0.,0.,1.));
#6004=DIRECTION('',(0.,0.,1.));
#6005=DIRECTION('center_axis',(0.,0.,1.));
#6006=DIRECTION('ref_axis',(-0.999501221021657,0.0315802022827165,0.));
#6007=DIRECTION('center_axis',(0.,0.,1.));
#6008=DIRECTION('ref_axis',(-0.999501221021657,0.0315802022827165,0.));
#6009=DIRECTION('center_axis',(0.,0.,1.));
#6010=DIRECTION('ref_axis',(-0.999501221021657,0.0315802022827165,0.));
#6011=DIRECTION('',(0.,0.,1.));
#6012=DIRECTION('',(0.,0.,1.));
#6013=DIRECTION('center_axis',(0.,0.,1.));
#6014=DIRECTION('ref_axis',(-0.940823330106451,0.338897420361099,0.));
#6015=DIRECTION('center_axis',(0.,0.,1.));
#6016=DIRECTION('ref_axis',(-0.940823330106451,0.338897420361099,0.));
#6017=DIRECTION('center_axis',(0.,0.,1.));
#6018=DIRECTION('ref_axis',(-0.940823330106451,0.338897420361099,0.));
#6019=DIRECTION('',(0.,0.,1.));
#6020=DIRECTION('',(0.,0.,1.));
#6021=DIRECTION('center_axis',(0.,0.,1.));
#6022=DIRECTION('ref_axis',(-0.790051096538837,0.613040997697366,0.));
#6023=DIRECTION('center_axis',(0.,0.,1.));
#6024=DIRECTION('ref_axis',(-0.790051096538837,0.613040997697366,0.));
#6025=DIRECTION('center_axis',(0.,0.,1.));
#6026=DIRECTION('ref_axis',(-0.790051096538837,0.613040997697366,0.));
#6027=DIRECTION('',(0.,0.,1.));
#6028=DIRECTION('',(0.,0.,1.));
#6029=DIRECTION('center_axis',(0.,0.,1.));
#6030=DIRECTION('ref_axis',(-0.561943157032333,0.827175850871225,0.));
#6031=DIRECTION('center_axis',(0.,0.,1.));
#6032=DIRECTION('ref_axis',(-0.561943157032333,0.827175850871225,0.));
#6033=DIRECTION('center_axis',(0.,0.,1.));
#6034=DIRECTION('ref_axis',(-0.561943157032333,0.827175850871225,0.));
#6035=DIRECTION('',(0.,0.,1.));
#6036=DIRECTION('',(0.,0.,1.));
#6037=DIRECTION('center_axis',(0.,0.,1.));
#6038=DIRECTION('ref_axis',(-0.278828306027306,0.960340968488767,0.));
#6039=DIRECTION('center_axis',(0.,0.,1.));
#6040=DIRECTION('ref_axis',(-0.278828306027306,0.960340968488767,0.));
#6041=DIRECTION('center_axis',(0.,0.,1.));
#6042=DIRECTION('ref_axis',(-0.278828306027306,0.960340968488767,0.));
#6043=DIRECTION('',(0.,0.,1.));
#6044=DIRECTION('',(0.,0.,1.));
#6045=DIRECTION('center_axis',(0.,0.,1.));
#6046=DIRECTION('ref_axis',(0.0315802022827164,0.999501221021657,0.));
#6047=DIRECTION('center_axis',(0.,0.,1.));
#6048=DIRECTION('ref_axis',(0.0315802022827164,0.999501221021657,0.));
#6049=DIRECTION('center_axis',(0.,0.,1.));
#6050=DIRECTION('ref_axis',(0.0315802022827164,0.999501221021657,0.));
#6051=DIRECTION('',(0.,0.,1.));
#6052=DIRECTION('',(0.,0.,1.));
#6053=DIRECTION('center_axis',(0.,0.,1.));
#6054=DIRECTION('ref_axis',(0.338897420361099,0.940823330106451,0.));
#6055=DIRECTION('center_axis',(0.,0.,1.));
#6056=DIRECTION('ref_axis',(0.338897420361099,0.940823330106451,0.));
#6057=DIRECTION('center_axis',(0.,0.,1.));
#6058=DIRECTION('ref_axis',(0.338897420361099,0.940823330106451,0.));
#6059=DIRECTION('',(0.,0.,1.));
#6060=DIRECTION('',(0.,0.,1.));
#6061=DIRECTION('center_axis',(0.,0.,1.));
#6062=DIRECTION('ref_axis',(0.613040997697366,0.790051096538837,0.));
#6063=DIRECTION('center_axis',(0.,0.,1.));
#6064=DIRECTION('ref_axis',(0.613040997697366,0.790051096538837,0.));
#6065=DIRECTION('center_axis',(0.,0.,1.));
#6066=DIRECTION('ref_axis',(0.613040997697366,0.790051096538837,0.));
#6067=DIRECTION('',(0.,0.,1.));
#6068=DIRECTION('',(0.,0.,1.));
#6069=DIRECTION('center_axis',(0.,0.,1.));
#6070=DIRECTION('ref_axis',(0.827175850871225,0.561943157032333,0.));
#6071=DIRECTION('center_axis',(0.,0.,1.));
#6072=DIRECTION('ref_axis',(0.827175850871225,0.561943157032333,0.));
#6073=DIRECTION('center_axis',(0.,0.,1.));
#6074=DIRECTION('ref_axis',(0.827175850871225,0.561943157032333,0.));
#6075=DIRECTION('',(0.,0.,1.));
#6076=DIRECTION('',(0.,0.,1.));
#6077=DIRECTION('center_axis',(0.,0.,1.));
#6078=DIRECTION('ref_axis',(0.960340968488767,0.278828306027306,0.));
#6079=DIRECTION('center_axis',(0.,0.,1.));
#6080=DIRECTION('ref_axis',(0.960340968488767,0.278828306027306,0.));
#6081=DIRECTION('center_axis',(0.,0.,1.));
#6082=DIRECTION('ref_axis',(0.960340968488767,0.278828306027306,0.));
#6083=DIRECTION('',(0.,0.,1.));
#6084=DIRECTION('center_axis',(0.,0.,1.));
#6085=DIRECTION('ref_axis',(1.,0.,0.));
#6086=DIRECTION('center_axis',(0.,0.,1.));
#6087=DIRECTION('ref_axis',(1.,0.,0.));
#6088=DIRECTION('center_axis',(0.,0.,1.));
#6089=DIRECTION('ref_axis',(1.,0.,0.));
#6090=DIRECTION('center_axis',(0.,0.,1.));
#6091=DIRECTION('ref_axis',(1.,0.,0.));
#6092=DIRECTION('center_axis',(0.,0.,1.));
#6093=DIRECTION('ref_axis',(1.,0.,0.));
#6094=DIRECTION('center_axis',(0.,0.,1.));
#6095=DIRECTION('ref_axis',(1.,0.,0.));
#6096=DIRECTION('center_axis',(0.,0.,1.));
#6097=DIRECTION('ref_axis',(1.,0.,0.));
#6098=DIRECTION('center_axis',(0.,0.,1.));
#6099=DIRECTION('ref_axis',(1.,0.,0.));
#6100=DIRECTION('center_axis',(0.,0.,1.));
#6101=DIRECTION('ref_axis',(1.,0.,0.));
#6102=DIRECTION('center_axis',(0.,0.,1.));
#6103=DIRECTION('ref_axis',(1.,0.,0.));
#6104=DIRECTION('center_axis',(0.,0.,1.));
#6105=DIRECTION('ref_axis',(1.,0.,0.));
#6106=DIRECTION('center_axis',(0.,0.,1.));
#6107=DIRECTION('ref_axis',(1.,0.,0.));
#6108=DIRECTION('center_axis',(0.,0.,1.));
#6109=DIRECTION('ref_axis',(1.,0.,0.));
#6110=DIRECTION('center_axis',(0.,0.,1.));
#6111=DIRECTION('ref_axis',(1.,0.,0.));
#6112=DIRECTION('center_axis',(0.,0.,1.));
#6113=DIRECTION('ref_axis',(1.,0.,0.));
#6114=DIRECTION('center_axis',(0.,0.,1.));
#6115=DIRECTION('ref_axis',(1.,0.,0.));
#6116=DIRECTION('center_axis',(0.,0.,1.));
#6117=DIRECTION('ref_axis',(1.,0.,0.));
#6118=DIRECTION('center_axis',(0.,0.,1.));
#6119=DIRECTION('ref_axis',(1.,0.,0.));
#6120=DIRECTION('center_axis',(0.,0.,1.));
#6121=DIRECTION('ref_axis',(1.,0.,0.));
#6122=DIRECTION('center_axis',(0.,0.,-1.));
#6123=DIRECTION('ref_axis',(-0.617203264866994,-0.786803742897505,0.));
#6124=DIRECTION('',(0.995637266659949,0.0933082699330836,0.));
#6125=DIRECTION('center_axis',(0.,0.,1.));
#6126=DIRECTION('ref_axis',(0.999501221021657,-0.0315802022827163,0.));
#6127=DIRECTION('',(0.995637266659949,-0.0933082699330836,0.));
#6128=DIRECTION('center_axis',(0.,0.,-1.));
#6129=DIRECTION('ref_axis',(-0.617203264866994,0.786803742897505,0.));
#6130=DIRECTION('center_axis',(0.,0.,1.));
#6131=DIRECTION('ref_axis',(1.,0.,0.));
#6132=DIRECTION('center_axis',(0.,0.,1.));
#6133=DIRECTION('ref_axis',(1.,0.,0.));
#6134=DIRECTION('center_axis',(0.,0.,1.));
#6135=DIRECTION('ref_axis',(1.,0.,0.));
#6136=DIRECTION('center_axis',(0.,0.,1.));
#6137=DIRECTION('ref_axis',(1.,0.,0.));
#6138=DIRECTION('center_axis',(0.,0.,-1.));
#6139=DIRECTION('ref_axis',(-0.617203264866994,0.786803742897505,0.));
#6140=DIRECTION('',(0.995637266659949,-0.0933082699330836,0.));
#6141=DIRECTION('center_axis',(0.,0.,1.));
#6142=DIRECTION('ref_axis',(0.999501221021657,-0.0315802022827163,0.));
#6143=DIRECTION('',(-0.995637266659949,-0.0933082699330836,0.));
#6144=DIRECTION('center_axis',(0.,0.,-1.));
#6145=DIRECTION('ref_axis',(-0.617203264866994,-0.786803742897505,0.));
#6146=DIRECTION('center_axis',(0.,0.,1.));
#6147=DIRECTION('ref_axis',(1.,0.,0.));
#6148=DIRECTION('center_axis',(0.,0.,1.));
#6149=DIRECTION('ref_axis',(1.,0.,0.));
#6150=DIRECTION('center_axis',(0.,0.,1.));
#6151=DIRECTION('ref_axis',(1.,0.,0.));
#6152=DIRECTION('center_axis',(0.,0.,1.));
#6153=DIRECTION('ref_axis',(1.,0.,0.));
#6154=DIRECTION('center_axis',(0.,0.,1.));
#6155=DIRECTION('ref_axis',(1.,0.,0.));
#6156=DIRECTION('center_axis',(0.,0.,1.));
#6157=DIRECTION('ref_axis',(1.,0.,0.));
#6158=DIRECTION('center_axis',(0.,0.,1.));
#6159=DIRECTION('ref_axis',(1.,0.,0.));
#6160=DIRECTION('center_axis',(0.,0.,1.));
#6161=DIRECTION('ref_axis',(1.,0.,0.));
#6162=DIRECTION('center_axis',(0.,0.,1.));
#6163=DIRECTION('ref_axis',(1.,0.,0.));
#6164=DIRECTION('center_axis',(0.,0.,1.));
#6165=DIRECTION('ref_axis',(1.,0.,0.));
#6166=DIRECTION('center_axis',(0.,0.,1.));
#6167=DIRECTION('ref_axis',(1.,0.,0.));
#6168=DIRECTION('center_axis',(0.,0.,1.));
#6169=DIRECTION('ref_axis',(1.,0.,0.));
#6170=DIRECTION('center_axis',(0.,0.,1.));
#6171=DIRECTION('ref_axis',(1.,0.,0.));
#6172=DIRECTION('center_axis',(0.,0.,1.));
#6173=DIRECTION('ref_axis',(1.,0.,0.));
#6174=DIRECTION('center_axis',(0.,0.,1.));
#6175=DIRECTION('ref_axis',(1.,0.,0.));
#6176=DIRECTION('center_axis',(0.,0.,1.));
#6177=DIRECTION('ref_axis',(1.,0.,0.));
#6178=DIRECTION('center_axis',(0.,0.,1.));
#6179=DIRECTION('ref_axis',(1.,0.,0.));
#6180=DIRECTION('center_axis',(0.,0.,1.));
#6181=DIRECTION('ref_axis',(1.,0.,0.));
#6182=DIRECTION('center_axis',(0.,0.,1.));
#6183=DIRECTION('ref_axis',(1.,0.,0.));
#6184=DIRECTION('center_axis',(0.,0.,1.));
#6185=DIRECTION('ref_axis',(1.,0.,0.));
#6186=DIRECTION('',(0.,0.,1.));
#6187=DIRECTION('center_axis',(0.,0.,1.));
#6188=DIRECTION('ref_axis',(1.,0.,0.));
#6189=DIRECTION('center_axis',(0.,0.,1.));
#6190=DIRECTION('ref_axis',(1.,0.,0.));
#6191=DIRECTION('center_axis',(0.,0.,1.));
#6192=DIRECTION('ref_axis',(1.,0.,0.));
#6193=DIRECTION('center_axis',(0.,0.,1.));
#6194=DIRECTION('ref_axis',(1.,0.,0.));
#6195=DIRECTION('center_axis',(0.,0.,1.));
#6196=DIRECTION('ref_axis',(1.,0.,0.));
#6197=DIRECTION('center_axis',(0.,0.,1.));
#6198=DIRECTION('ref_axis',(1.,0.,0.));
#6199=DIRECTION('center_axis',(0.,0.,1.));
#6200=DIRECTION('ref_axis',(1.,0.,0.));
#6201=DIRECTION('center_axis',(0.,0.,1.));
#6202=DIRECTION('ref_axis',(1.,0.,0.));
#6203=DIRECTION('center_axis',(0.,0.,1.));
#6204=DIRECTION('ref_axis',(1.,0.,0.));
#6205=DIRECTION('center_axis',(0.,0.,1.));
#6206=DIRECTION('ref_axis',(1.,0.,0.));
#6207=DIRECTION('center_axis',(0.,0.,1.));
#6208=DIRECTION('ref_axis',(1.,0.,0.));
#6209=DIRECTION('center_axis',(0.,0.,1.));
#6210=DIRECTION('ref_axis',(1.,0.,0.));
#6211=DIRECTION('center_axis',(0.,0.,1.));
#6212=DIRECTION('ref_axis',(1.,0.,0.));
#6213=DIRECTION('center_axis',(0.,0.,1.));
#6214=DIRECTION('ref_axis',(1.,0.,0.));
#6215=DIRECTION('center_axis',(0.,0.,1.));
#6216=DIRECTION('ref_axis',(1.,0.,0.));
#6217=DIRECTION('center_axis',(0.,0.,1.));
#6218=DIRECTION('ref_axis',(1.,0.,0.));
#6219=DIRECTION('center_axis',(0.,0.,1.));
#6220=DIRECTION('ref_axis',(1.,0.,0.));
#6221=DIRECTION('center_axis',(0.,0.,1.));
#6222=DIRECTION('ref_axis',(1.,0.,0.));
#6223=DIRECTION('center_axis',(0.,0.,-1.));
#6224=DIRECTION('ref_axis',(-0.617203264866994,-0.786803742897505,0.));
#6225=DIRECTION('',(0.,0.,-1.));
#6226=DIRECTION('center_axis',(-0.0933082699330836,0.995637266659949,0.));
#6227=DIRECTION('ref_axis',(-0.995637266659949,-0.0933082699330836,0.));
#6228=DIRECTION('',(0.,0.,1.));
#6229=DIRECTION('center_axis',(0.,0.,1.));
#6230=DIRECTION('ref_axis',(-0.617203264866994,0.786803742897505,0.));
#6231=DIRECTION('',(0.,0.,1.));
#6232=DIRECTION('',(0.,0.,-1.));
#6233=DIRECTION('center_axis',(-0.0933082699330836,-0.995637266659949,0.));
#6234=DIRECTION('ref_axis',(0.995637266659949,-0.0933082699330836,0.));
#6235=DIRECTION('',(0.,0.,1.));
#6236=DIRECTION('',(0.,0.,1.));
#6237=DIRECTION('center_axis',(0.,0.,1.));
#6238=DIRECTION('ref_axis',(0.999501221021657,-0.0315802022827163,0.));
#6239=DIRECTION('',(0.,0.,1.));
#6240=DIRECTION('center_axis',(0.,0.,1.));
#6241=DIRECTION('ref_axis',(1.,0.,0.));
#6242=DIRECTION('axis',(0.,0.,1.));
#6243=DIRECTION('refdir',(1.,0.,0.));
#6244=DIRECTION('center_axis',(-7.86407975776121E-17,0.,1.));
#6245=DIRECTION('ref_axis',(-1.,0.,-7.86407975776121E-17));
#6246=DIRECTION('center_axis',(-7.86407975776121E-17,0.,1.));
#6247=DIRECTION('ref_axis',(-1.,0.,-7.86407975776121E-17));
#6248=DIRECTION('',(-0.739940073395942,-9.06165242445198E-17,-0.672672793996315));
#6249=DIRECTION('center_axis',(7.86407975776121E-17,0.,-1.));
#6250=DIRECTION('ref_axis',(-1.,0.,-7.86407975776121E-17));
#6251=DIRECTION('center_axis',(7.86407975776121E-17,0.,-1.));
#6252=DIRECTION('ref_axis',(-1.,0.,-8.96154192009005E-17));
#6253=DIRECTION('center_axis',(-7.86407975776121E-17,0.,1.));
#6254=DIRECTION('ref_axis',(-1.,0.,-7.86407975776121E-17));
#6255=DIRECTION('center_axis',(1.22464679914735E-16,1.,9.63072010358176E-33));
#6256=DIRECTION('ref_axis',(1.,-1.22464679914735E-16,1.12019274001126E-16));
#6257=DIRECTION('center_axis',(0.,0.,-1.));
#6258=DIRECTION('ref_axis',(-1.,6.12323399573677E-17,0.));
#6259=DIRECTION('center_axis',(-7.86407975776121E-17,0.,1.));
#6260=DIRECTION('ref_axis',(-1.,0.,-7.86407975776121E-17));
#6261=DIRECTION('center_axis',(7.86407975776121E-17,0.,-1.));
#6262=DIRECTION('ref_axis',(1.,0.,7.86407975776121E-17));
#6263=DIRECTION('',(-0.70710678118658,-8.65956056235534E-17,-0.707106781186515));
#6264=DIRECTION('center_axis',(7.86407975776121E-17,0.,-1.));
#6265=DIRECTION('ref_axis',(-1.,0.,-7.86407975776121E-17));
#6266=DIRECTION('',(-7.86407975776121E-17,0.,1.));
#6267=DIRECTION('center_axis',(0.25,0.433012701892219,-0.866025403784439));
#6268=DIRECTION('ref_axis',(0.866025403784439,-0.5,2.49215522988657E-16));
#6269=DIRECTION('',(-0.774596669241483,-0.447213595499958,-0.447213595499958));
#6270=DIRECTION('',(0.866025403784439,-0.5,6.81049284760846E-17));
#6271=DIRECTION('',(-1.1466334093198E-16,-0.894427190999916,-0.447213595499958));
#6272=DIRECTION('center_axis',(-0.25,0.433012701892219,-0.866025403784439));
#6273=DIRECTION('ref_axis',(0.866025403784439,0.5,-1.73385880213439E-16));
#6274=DIRECTION('',(0.866025403784439,0.5,6.81049284760846E-17));
#6275=DIRECTION('',(0.774596669241484,-0.447213595499958,-0.447213595499958));
#6276=DIRECTION('center_axis',(-0.5,-1.92296268638357E-16,-0.866025403784439));
#6277=DIRECTION('ref_axis',(-3.84592537276713E-16,1.,-4.40476560101798E-31));
#6278=DIRECTION('',(-3.84592537276713E-16,1.,-3.02446638738394E-32));
#6279=DIRECTION('',(0.774596669241483,0.447213595499958,-0.447213595499958));
#6280=DIRECTION('center_axis',(-0.25,-0.433012701892219,-0.866025403784439));
#6281=DIRECTION('ref_axis',(-0.866025403784438,0.5,-2.09031490959634E-17));
#6282=DIRECTION('',(-0.866025403784438,0.5,-6.81049284760846E-17));
#6283=DIRECTION('',(6.87980045591882E-16,0.894427190999916,-0.447213595499958));
#6284=DIRECTION('center_axis',(0.25,-0.43301270189222,-0.866025403784438));
#6285=DIRECTION('ref_axis',(-0.866025403784439,-0.499999999999999,-1.78830203614062E-16));
#6286=DIRECTION('',(-0.866025403784439,-0.499999999999999,-6.81049284760846E-17));
#6287=DIRECTION('',(-0.774596669241483,0.447213595499959,-0.447213595499958));
#6288=DIRECTION('center_axis',(0.5,0.,-0.866025403784438));
#6289=DIRECTION('ref_axis',(0.,-1.,0.));
#6290=DIRECTION('',(0.,-1.,0.));
#6291=DIRECTION('center_axis',(0.5,0.866025403784439,5.78241158658936E-17));
#6292=DIRECTION('ref_axis',(0.866025403784439,-0.5,6.81049284760846E-17));
#6293=DIRECTION('',(0.866025403784439,-0.5,6.81049284760818E-17));
#6294=DIRECTION('',(1.15648231731787E-16,0.,-1.));
#6295=DIRECTION('',(1.15648231731787E-16,0.,-1.));
#6296=DIRECTION('center_axis',(-0.5,0.866025403784439,-5.78241158658936E-17));
#6297=DIRECTION('ref_axis',(0.866025403784439,0.5,6.81049284760846E-17));
#6298=DIRECTION('',(0.866025403784439,0.5,6.81049284760818E-17));
#6299=DIRECTION('',(1.15648231731787E-16,0.,-1.));
#6300=DIRECTION('center_axis',(-1.,-3.84592537276713E-16,-1.15648231731787E-16));
#6301=DIRECTION('ref_axis',(-3.84592537276713E-16,1.,-3.02446638738394E-32));
#6302=DIRECTION('',(-3.84592537276713E-16,1.,-3.02446638738382E-32));
#6303=DIRECTION('',(1.15648231731787E-16,0.,-1.));
#6304=DIRECTION('center_axis',(-0.5,-0.866025403784439,-5.78241158658936E-17));
#6305=DIRECTION('ref_axis',(-0.866025403784439,0.5,-6.81049284760847E-17));
#6306=DIRECTION('',(-0.866025403784438,0.5,-6.81049284760818E-17));
#6307=DIRECTION('',(1.15648231731787E-16,0.,-1.));
#6308=DIRECTION('center_axis',(0.499999999999999,-0.866025403784439,5.78241158658935E-17));
#6309=DIRECTION('ref_axis',(-0.866025403784439,-0.499999999999999,-6.81049284760846E-17));
#6310=DIRECTION('',(-0.866025403784439,-0.499999999999999,-6.81049284760819E-17));
#6311=DIRECTION('',(1.15648231731787E-16,0.,-1.));
#6312=DIRECTION('center_axis',(1.,0.,1.15648231731787E-16));
#6313=DIRECTION('ref_axis',(0.,-1.,0.));
#6314=DIRECTION('',(0.,-1.,0.));
#6315=DIRECTION('center_axis',(-7.86407975776121E-17,0.,1.));
#6316=DIRECTION('ref_axis',(1.,0.,7.86407975776121E-17));
#6317=DIRECTION('center_axis',(7.86407975776121E-17,0.,-1.));
#6318=DIRECTION('ref_axis',(1.,0.,7.86407975776121E-17));
#6319=DIRECTION('center_axis',(7.86407975776121E-17,0.,-1.));
#6320=DIRECTION('ref_axis',(-1.,0.,-7.86407975776121E-17));
#6321=DIRECTION('',(-7.86407975776121E-17,0.,1.));
#6322=DIRECTION('center_axis',(7.86407975776121E-17,0.,-1.));
#6323=DIRECTION('ref_axis',(-1.,0.,-7.86407975776121E-17));
#6324=DIRECTION('axis',(0.,0.,1.));
#6325=DIRECTION('refdir',(1.,0.,0.));
#6326=DIRECTION('center_axis',(-7.86407975776121E-17,0.,1.));
#6327=DIRECTION('ref_axis',(-1.,0.,-7.86407975776121E-17));
#6328=DIRECTION('center_axis',(-7.86407975776121E-17,0.,1.));
#6329=DIRECTION('ref_axis',(-1.,0.,-7.86407975776121E-17));
#6330=DIRECTION('',(-0.739940073395942,-9.06165242445198E-17,-0.672672793996315));
#6331=DIRECTION('center_axis',(7.86407975776121E-17,0.,-1.));
#6332=DIRECTION('ref_axis',(-1.,0.,-7.86407975776121E-17));
#6333=DIRECTION('center_axis',(7.86407975776121E-17,0.,-1.));
#6334=DIRECTION('ref_axis',(-1.,0.,-8.96154192009005E-17));
#6335=DIRECTION('center_axis',(-7.86407975776121E-17,0.,1.));
#6336=DIRECTION('ref_axis',(-1.,0.,-7.86407975776121E-17));
#6337=DIRECTION('center_axis',(1.22464679914735E-16,1.,9.63072010358176E-33));
#6338=DIRECTION('ref_axis',(1.,-1.22464679914735E-16,1.12019274001126E-16));
#6339=DIRECTION('center_axis',(0.,0.,-1.));
#6340=DIRECTION('ref_axis',(-1.,6.12323399573677E-17,0.));
#6341=DIRECTION('center_axis',(-7.86407975776121E-17,0.,1.));
#6342=DIRECTION('ref_axis',(-1.,0.,-7.86407975776121E-17));
#6343=DIRECTION('center_axis',(7.86407975776121E-17,0.,-1.));
#6344=DIRECTION('ref_axis',(1.,0.,7.86407975776121E-17));
#6345=DIRECTION('',(-0.70710678118658,-8.65956056235534E-17,-0.707106781186515));
#6346=DIRECTION('center_axis',(7.86407975776121E-17,0.,-1.));
#6347=DIRECTION('ref_axis',(-1.,0.,-7.86407975776121E-17));
#6348=DIRECTION('',(-7.86407975776121E-17,0.,1.));
#6349=DIRECTION('center_axis',(0.25,0.433012701892219,-0.866025403784439));
#6350=DIRECTION('ref_axis',(0.866025403784439,-0.5,2.49215522988657E-16));
#6351=DIRECTION('',(-0.774596669241483,-0.447213595499958,-0.447213595499958));
#6352=DIRECTION('',(0.866025403784439,-0.5,6.81049284760846E-17));
#6353=DIRECTION('',(-1.1466334093198E-16,-0.894427190999916,-0.447213595499958));
#6354=DIRECTION('center_axis',(-0.25,0.433012701892219,-0.866025403784439));
#6355=DIRECTION('ref_axis',(0.866025403784439,0.5,-1.73385880213439E-16));
#6356=DIRECTION('',(0.866025403784439,0.5,6.81049284760846E-17));
#6357=DIRECTION('',(0.774596669241484,-0.447213595499958,-0.447213595499958));
#6358=DIRECTION('center_axis',(-0.5,-1.92296268638357E-16,-0.866025403784439));
#6359=DIRECTION('ref_axis',(-3.84592537276713E-16,1.,-4.40476560101798E-31));
#6360=DIRECTION('',(-3.84592537276713E-16,1.,-3.02446638738394E-32));
#6361=DIRECTION('',(0.774596669241483,0.447213595499958,-0.447213595499958));
#6362=DIRECTION('center_axis',(-0.25,-0.433012701892219,-0.866025403784439));
#6363=DIRECTION('ref_axis',(-0.866025403784438,0.5,-2.09031490959634E-17));
#6364=DIRECTION('',(-0.866025403784438,0.5,-6.81049284760846E-17));
#6365=DIRECTION('',(6.87980045591882E-16,0.894427190999916,-0.447213595499958));
#6366=DIRECTION('center_axis',(0.25,-0.43301270189222,-0.866025403784438));
#6367=DIRECTION('ref_axis',(-0.866025403784439,-0.499999999999999,-1.78830203614062E-16));
#6368=DIRECTION('',(-0.866025403784439,-0.499999999999999,-6.81049284760846E-17));
#6369=DIRECTION('',(-0.774596669241483,0.447213595499959,-0.447213595499958));
#6370=DIRECTION('center_axis',(0.5,0.,-0.866025403784438));
#6371=DIRECTION('ref_axis',(0.,-1.,0.));
#6372=DIRECTION('',(0.,-1.,0.));
#6373=DIRECTION('center_axis',(0.5,0.866025403784439,5.78241158658936E-17));
#6374=DIRECTION('ref_axis',(0.866025403784439,-0.5,6.81049284760846E-17));
#6375=DIRECTION('',(0.866025403784439,-0.5,6.81049284760818E-17));
#6376=DIRECTION('',(1.15648231731787E-16,0.,-1.));
#6377=DIRECTION('',(1.15648231731787E-16,0.,-1.));
#6378=DIRECTION('center_axis',(-0.5,0.866025403784439,-5.78241158658936E-17));
#6379=DIRECTION('ref_axis',(0.866025403784439,0.5,6.81049284760846E-17));
#6380=DIRECTION('',(0.866025403784439,0.5,6.81049284760818E-17));
#6381=DIRECTION('',(1.15648231731787E-16,0.,-1.));
#6382=DIRECTION('center_axis',(-1.,-3.84592537276713E-16,-1.15648231731787E-16));
#6383=DIRECTION('ref_axis',(-3.84592537276713E-16,1.,-3.02446638738394E-32));
#6384=DIRECTION('',(-3.84592537276713E-16,1.,-3.02446638738382E-32));
#6385=DIRECTION('',(1.15648231731787E-16,0.,-1.));
#6386=DIRECTION('center_axis',(-0.5,-0.866025403784439,-5.78241158658936E-17));
#6387=DIRECTION('ref_axis',(-0.866025403784439,0.5,-6.81049284760847E-17));
#6388=DIRECTION('',(-0.866025403784438,0.5,-6.81049284760818E-17));
#6389=DIRECTION('',(1.15648231731787E-16,0.,-1.));
#6390=DIRECTION('center_axis',(0.499999999999999,-0.866025403784439,5.78241158658935E-17));
#6391=DIRECTION('ref_axis',(-0.866025403784439,-0.499999999999999,-6.81049284760846E-17));
#6392=DIRECTION('',(-0.866025403784439,-0.499999999999999,-6.81049284760819E-17));
#6393=DIRECTION('',(1.15648231731787E-16,0.,-1.));
#6394=DIRECTION('center_axis',(1.,0.,1.15648231731787E-16));
#6395=DIRECTION('ref_axis',(0.,-1.,0.));
#6396=DIRECTION('',(0.,-1.,0.));
#6397=DIRECTION('center_axis',(-7.86407975776121E-17,0.,1.));
#6398=DIRECTION('ref_axis',(1.,0.,7.86407975776121E-17));
#6399=DIRECTION('center_axis',(7.86407975776121E-17,0.,-1.));
#6400=DIRECTION('ref_axis',(1.,0.,7.86407975776121E-17));
#6401=DIRECTION('center_axis',(7.86407975776121E-17,0.,-1.));
#6402=DIRECTION('ref_axis',(-1.,0.,-7.86407975776121E-17));
#6403=DIRECTION('',(-7.86407975776121E-17,0.,1.));
#6404=DIRECTION('center_axis',(7.86407975776121E-17,0.,-1.));
#6405=DIRECTION('ref_axis',(-1.,0.,-7.86407975776121E-17));
#6406=DIRECTION('axis',(0.,0.,1.));
#6407=DIRECTION('refdir',(1.,0.,0.));
#6408=DIRECTION('center_axis',(0.,0.,-1.));
#6409=DIRECTION('ref_axis',(-1.,0.,0.));
#6410=DIRECTION('center_axis',(0.,0.,1.));
#6411=DIRECTION('ref_axis',(-1.,0.,0.));
#6412=DIRECTION('',(0.,0.,1.));
#6413=DIRECTION('center_axis',(0.,0.,1.));
#6414=DIRECTION('ref_axis',(-1.,0.,0.));
#6415=DIRECTION('center_axis',(0.,0.,1.));
#6416=DIRECTION('ref_axis',(1.,0.,0.));
#6417=DIRECTION('center_axis',(0.,0.,1.));
#6418=DIRECTION('ref_axis',(1.,0.,0.));
#6419=DIRECTION('center_axis',(0.,0.,1.));
#6420=DIRECTION('ref_axis',(1.,0.,0.));
#6421=DIRECTION('center_axis',(0.,0.,1.));
#6422=DIRECTION('ref_axis',(1.,0.,0.));
#6423=DIRECTION('center_axis',(-1.22464679914735E-16,1.,0.));
#6424=DIRECTION('ref_axis',(-1.,-1.22464679914735E-16,0.));
#6425=DIRECTION('center_axis',(0.,0.,1.));
#6426=DIRECTION('ref_axis',(1.,0.,0.));
#6427=DIRECTION('center_axis',(0.,0.,1.));
#6428=DIRECTION('ref_axis',(1.,0.,0.));
#6429=DIRECTION('',(0.,0.,-1.));
#6430=DIRECTION('center_axis',(0.,0.,-1.));
#6431=DIRECTION('ref_axis',(-1.,0.,0.));
#6432=DIRECTION('center_axis',(0.,0.,1.));
#6433=DIRECTION('ref_axis',(1.,0.,0.));
#6434=DIRECTION('center_axis',(0.,0.,1.));
#6435=DIRECTION('ref_axis',(1.,0.,0.));
#6436=DIRECTION('center_axis',(0.,0.,1.));
#6437=DIRECTION('ref_axis',(1.,0.,0.));
#6438=DIRECTION('',(0.,0.,-1.));
#6439=DIRECTION('center_axis',(0.,0.,1.));
#6440=DIRECTION('ref_axis',(1.,0.,0.));
#6441=DIRECTION('center_axis',(0.,0.,1.));
#6442=DIRECTION('ref_axis',(-1.,0.,0.));
#6443=DIRECTION('axis',(0.,0.,1.));
#6444=DIRECTION('refdir',(1.,0.,0.));
#6445=DIRECTION('center_axis',(0.,0.,1.));
#6446=DIRECTION('ref_axis',(1.,0.,0.));
#6447=DIRECTION('center_axis',(0.,0.,-1.));
#6448=DIRECTION('ref_axis',(-1.,1.22464679914735E-16,0.));
#6449=DIRECTION('center_axis',(1.22464679914735E-16,-1.,0.));
#6450=DIRECTION('ref_axis',(-1.,-1.22464679914735E-16,0.));
#6451=DIRECTION('center_axis',(0.,0.,1.));
#6452=DIRECTION('ref_axis',(-1.,1.22464679914735E-16,0.));
#6453=DIRECTION('center_axis',(0.,0.,1.));
#6454=DIRECTION('ref_axis',(1.,0.,0.));
#6455=DIRECTION('',(0.,0.,-1.));
#6456=DIRECTION('center_axis',(0.,0.,1.));
#6457=DIRECTION('ref_axis',(1.,0.,0.));
#6458=DIRECTION('center_axis',(0.,0.,1.));
#6459=DIRECTION('ref_axis',(1.,0.,0.));
#6460=DIRECTION('center_axis',(0.,0.,1.));
#6461=DIRECTION('ref_axis',(1.,0.,0.));
#6462=DIRECTION('center_axis',(0.,0.,1.));
#6463=DIRECTION('ref_axis',(1.,0.,0.));
#6464=DIRECTION('center_axis',(0.,0.,-1.));
#6465=DIRECTION('ref_axis',(-1.,1.22464679914735E-16,0.));
#6466=DIRECTION('center_axis',(1.22464679914735E-16,-1.,0.));
#6467=DIRECTION('ref_axis',(-1.,-1.22464679914735E-16,0.));
#6468=DIRECTION('center_axis',(0.,0.,1.));
#6469=DIRECTION('ref_axis',(-1.,1.22464679914735E-16,0.));
#6470=DIRECTION('center_axis',(0.,0.,1.));
#6471=DIRECTION('ref_axis',(1.,0.,0.));
#6472=DIRECTION('center_axis',(0.,0.,-1.));
#6473=DIRECTION('ref_axis',(-1.,1.22464679914735E-16,0.));
#6474=DIRECTION('center_axis',(0.,0.,1.));
#6475=DIRECTION('ref_axis',(1.,0.,0.));
#6476=DIRECTION('center_axis',(0.,0.,1.));
#6477=DIRECTION('ref_axis',(1.,0.,0.));
#6478=DIRECTION('',(0.,0.,1.));
#6479=DIRECTION('center_axis',(0.,0.,1.));
#6480=DIRECTION('ref_axis',(1.,0.,0.));
#6481=DIRECTION('center_axis',(1.22464679914735E-16,-1.,0.));
#6482=DIRECTION('ref_axis',(-1.,-1.22464679914735E-16,0.));
#6483=DIRECTION('center_axis',(0.,0.,1.));
#6484=DIRECTION('ref_axis',(-1.,1.22464679914735E-16,0.));
#6485=DIRECTION('center_axis',(0.,0.,1.));
#6486=DIRECTION('ref_axis',(1.,0.,0.));
#6487=DIRECTION('',(0.,0.,-1.));
#6488=DIRECTION('center_axis',(0.,0.,1.));
#6489=DIRECTION('ref_axis',(1.,0.,0.));
#6490=DIRECTION('center_axis',(0.,0.,1.));
#6491=DIRECTION('ref_axis',(1.,0.,0.));
#6492=DIRECTION('center_axis',(0.,0.,1.));
#6493=DIRECTION('ref_axis',(1.,0.,0.));
#6494=DIRECTION('center_axis',(0.,0.,1.));
#6495=DIRECTION('ref_axis',(1.,0.,0.));
#6496=DIRECTION('',(0.,0.,1.));
#6497=DIRECTION('center_axis',(0.,0.,1.));
#6498=DIRECTION('ref_axis',(1.,0.,0.));
#6499=DIRECTION('center_axis',(0.,0.,1.));
#6500=DIRECTION('ref_axis',(1.,0.,0.));
#6501=DIRECTION('center_axis',(-1.22464679914735E-16,1.,0.));
#6502=DIRECTION('ref_axis',(-1.,-1.22464679914735E-16,0.));
#6503=DIRECTION('center_axis',(0.,0.,-1.));
#6504=DIRECTION('ref_axis',(-1.,0.,0.));
#6505=DIRECTION('center_axis',(0.,0.,1.));
#6506=DIRECTION('ref_axis',(1.,0.,0.));
#6507=DIRECTION('center_axis',(0.,0.,1.));
#6508=DIRECTION('ref_axis',(1.,0.,0.));
#6509=DIRECTION('center_axis',(0.,0.,1.));
#6510=DIRECTION('ref_axis',(1.,0.,0.));
#6511=DIRECTION('',(0.,0.,-1.));
#6512=DIRECTION('center_axis',(0.,0.,-1.));
#6513=DIRECTION('ref_axis',(-1.,0.,0.));
#6514=DIRECTION('center_axis',(0.,0.,1.));
#6515=DIRECTION('ref_axis',(1.,0.,0.));
#6516=DIRECTION('center_axis',(0.,0.,1.));
#6517=DIRECTION('ref_axis',(1.,0.,0.));
#6518=DIRECTION('center_axis',(0.,0.,1.));
#6519=DIRECTION('ref_axis',(1.,0.,0.));
#6520=DIRECTION('',(0.,0.,1.));
#6521=DIRECTION('center_axis',(0.,0.,-1.));
#6522=DIRECTION('ref_axis',(-1.,0.,0.));
#6523=DIRECTION('center_axis',(0.,0.,1.));
#6524=DIRECTION('ref_axis',(1.,0.,0.));
#6525=DIRECTION('center_axis',(0.,0.,1.));
#6526=DIRECTION('ref_axis',(1.,0.,0.));
#6527=DIRECTION('center_axis',(0.,0.,1.));
#6528=DIRECTION('ref_axis',(1.,0.,0.));
#6529=DIRECTION('',(0.,0.,1.));
#6530=DIRECTION('center_axis',(0.,0.,-1.));
#6531=DIRECTION('ref_axis',(-1.,0.,0.));
#6532=DIRECTION('axis',(0.,0.,1.));
#6533=DIRECTION('refdir',(1.,0.,0.));
#6534=DIRECTION('center_axis',(0.,0.,1.));
#6535=DIRECTION('ref_axis',(-0.894892375881552,-0.446282013517317,0.));
#6536=DIRECTION('center_axis',(0.,0.,1.));
#6537=DIRECTION('ref_axis',(-0.79874874277943,0.601664728821858,0.));
#6538=DIRECTION('',(0.,0.,1.));
#6539=DIRECTION('center_axis',(0.,0.,1.));
#6540=DIRECTION('ref_axis',(-0.894892375881552,-0.446282013517317,0.));
#6541=DIRECTION('',(0.,0.,-1.));
#6542=DIRECTION('center_axis',(0.,0.,1.));
#6543=DIRECTION('ref_axis',(1.,-1.22464679914735E-16,0.));
#6544=DIRECTION('center_axis',(-0.601664728821861,0.798748742779428,-3.54715698049647E-15));
#6545=DIRECTION('ref_axis',(-0.798748742779428,-0.601664728821861,-1.85390118736899E-31));
#6546=DIRECTION('center_axis',(0.,0.,1.));
#6547=DIRECTION('ref_axis',(1.,1.22464679914735E-16,0.));
#6548=DIRECTION('center_axis',(-0.601664728821861,-0.798748742779428,-3.54715698049647E-15));
#6549=DIRECTION('ref_axis',(2.50378775993336E-30,-4.44089209850063E-15,
1.));
#6550=DIRECTION('center_axis',(0.,0.,-1.));
#6551=DIRECTION('ref_axis',(1.,1.22464679914735E-16,0.));
#6552=DIRECTION('center_axis',(0.185467508428577,-0.954822547310801,-0.232197559126295));
#6553=DIRECTION('ref_axis',(-0.595903538017452,-0.297176552148574,0.746046292284446));
#6554=DIRECTION('center_axis',(1.,0.,0.));
#6555=DIRECTION('ref_axis',(0.,-0.707106781186546,0.707106781186549));
#6556=DIRECTION('center_axis',(0.,0.,1.));
#6557=DIRECTION('ref_axis',(-0.894892375881552,0.446282013517317,0.));
#6558=DIRECTION('center_axis',(0.,0.,1.));
#6559=DIRECTION('ref_axis',(0.,1.,0.));
#6560=DIRECTION('',(0.,0.,1.));
#6561=DIRECTION('center_axis',(0.,0.,1.));
#6562=DIRECTION('ref_axis',(-0.894892375881552,0.446282013517317,0.));
#6563=DIRECTION('',(0.,0.,-1.));
#6564=DIRECTION('center_axis',(-0.185467508428577,-0.954822547310802,0.23219755912629));
#6565=DIRECTION('ref_axis',(-0.595903538017456,0.297176552148567,0.746046292284445));
#6566=DIRECTION('center_axis',(1.,0.,0.));
#6567=DIRECTION('ref_axis',(0.,0.707106781186546,0.707106781186549));
#6568=DIRECTION('center_axis',(0.,1.,0.));
#6569=DIRECTION('ref_axis',(1.,0.,0.));
#6570=DIRECTION('',(1.,0.,0.));
#6571=DIRECTION('',(0.,0.,1.));
#6572=DIRECTION('',(1.,0.,0.));
#6573=DIRECTION('',(0.,0.,1.));
#6574=DIRECTION('',(-1.,0.,0.));
#6575=DIRECTION('center_axis',(-1.,0.,0.));
#6576=DIRECTION('ref_axis',(0.,-0.707106781186547,0.707106781186548));
#6577=DIRECTION('center_axis',(1.,0.,0.));
#6578=DIRECTION('ref_axis',(0.,0.,1.));
#6579=DIRECTION('',(1.,0.,0.));
#6580=DIRECTION('center_axis',(0.,0.,-1.));
#6581=DIRECTION('ref_axis',(-1.,0.,0.));
#6582=DIRECTION('center_axis',(0.,0.,1.));
#6583=DIRECTION('ref_axis',(0.707106781186548,-0.707106781186547,0.));
#6584=DIRECTION('',(0.,1.,0.));
#6585=DIRECTION('center_axis',(0.,0.,1.));
#6586=DIRECTION('ref_axis',(0.707106781186548,0.707106781186547,0.));
#6587=DIRECTION('',(-1.,0.,0.));
#6588=DIRECTION('center_axis',(0.,0.,-1.));
#6589=DIRECTION('ref_axis',(-1.,0.,0.));
#6590=DIRECTION('center_axis',(1.,0.,0.));
#6591=DIRECTION('ref_axis',(0.,0.707106781186547,0.707106781186548));
#6592=DIRECTION('center_axis',(-1.,0.,0.));
#6593=DIRECTION('ref_axis',(0.,0.,1.));
#6594=DIRECTION('',(1.,0.,0.));
#6595=DIRECTION('center_axis',(0.,-1.,0.));
#6596=DIRECTION('ref_axis',(-1.,0.,0.));
#6597=DIRECTION('',(0.,0.,-1.));
#6598=DIRECTION('',(-1.,0.,0.));
#6599=DIRECTION('',(0.,0.,-1.));
#6600=DIRECTION('',(-1.,0.,0.));
#6601=DIRECTION('center_axis',(0.,0.,-1.));
#6602=DIRECTION('ref_axis',(1.,0.,0.));
#6603=DIRECTION('center_axis',(2.22044604925032E-15,1.,0.));
#6604=DIRECTION('ref_axis',(0.,0.,1.));
#6605=DIRECTION('center_axis',(0.,0.,-1.));
#6606=DIRECTION('ref_axis',(0.707106781186548,-0.707106781186547,0.));
#6607=DIRECTION('center_axis',(0.,-1.,0.));
#6608=DIRECTION('ref_axis',(0.707106781186547,0.,0.707106781186548));
#6609=DIRECTION('center_axis',(-2.22044604925032E-15,1.,0.));
#6610=DIRECTION('ref_axis',(0.,0.,1.));
#6611=DIRECTION('',(0.,-1.,0.));
#6612=DIRECTION('center_axis',(0.,0.,-1.));
#6613=DIRECTION('ref_axis',(1.,0.,0.));
#6614=DIRECTION('center_axis',(0.,0.,-1.));
#6615=DIRECTION('ref_axis',(0.707106781186548,0.707106781186547,0.));
#6616=DIRECTION('center_axis',(0.,0.,1.));
#6617=DIRECTION('ref_axis',(-1.,0.,0.));
#6618=DIRECTION('center_axis',(0.,0.,1.));
#6619=DIRECTION('ref_axis',(-1.,0.,0.));
#6620=DIRECTION('',(0.707106781186548,8.65956056235494E-17,0.707106781186547));
#6621=DIRECTION('center_axis',(0.,0.,1.));
#6622=DIRECTION('ref_axis',(-1.,0.,0.));
#6623=DIRECTION('center_axis',(0.,0.,-1.));
#6624=DIRECTION('ref_axis',(-1.,0.,0.));
#6625=DIRECTION('',(0.,0.,1.));
#6626=DIRECTION('center_axis',(0.,0.,1.));
#6627=DIRECTION('ref_axis',(0.707106781186548,-0.707106781186548,0.));
#6628=DIRECTION('center_axis',(0.,0.,-1.));
#6629=DIRECTION('ref_axis',(0.707106781186548,-0.707106781186548,0.));
#6630=DIRECTION('',(0.,0.,-1.));
#6631=DIRECTION('center_axis',(-1.,0.,0.));
#6632=DIRECTION('ref_axis',(0.,1.,0.));
#6633=DIRECTION('',(0.,1.,0.));
#6634=DIRECTION('',(0.,0.,1.));
#6635=DIRECTION('center_axis',(0.,0.,1.));
#6636=DIRECTION('ref_axis',(0.707106781186548,0.707106781186548,0.));
#6637=DIRECTION('center_axis',(0.,0.,-1.));
#6638=DIRECTION('ref_axis',(0.707106781186548,0.707106781186548,0.));
#6639=DIRECTION('center_axis',(0.,0.,1.));
#6640=DIRECTION('ref_axis',(1.,-1.22464679914735E-16,0.));
#6641=DIRECTION('center_axis',(0.,0.,1.));
#6642=DIRECTION('ref_axis',(-1.,0.,0.));
#6643=DIRECTION('center_axis',(0.,0.,1.));
#6644=DIRECTION('ref_axis',(1.,0.,0.));
#6645=DIRECTION('center_axis',(0.,0.,-1.));
#6646=DIRECTION('ref_axis',(1.,0.,0.));
#6647=DIRECTION('',(0.,0.,1.));
#6648=DIRECTION('center_axis',(0.,0.,1.));
#6649=DIRECTION('ref_axis',(1.,0.,0.));
#6650=DIRECTION('center_axis',(0.,0.,1.));
#6651=DIRECTION('ref_axis',(1.,0.,0.));
#6652=DIRECTION('center_axis',(0.,0.,1.));
#6653=DIRECTION('ref_axis',(1.,0.,0.));
#6654=DIRECTION('',(0.,0.,-1.));
#6655=DIRECTION('center_axis',(0.,0.,-1.));
#6656=DIRECTION('ref_axis',(1.,0.,0.));
#6657=DIRECTION('center_axis',(0.,0.,-1.));
#6658=DIRECTION('ref_axis',(0.894892375881552,-0.446282013517317,0.));
#6659=DIRECTION('center_axis',(0.,0.,-1.));
#6660=DIRECTION('ref_axis',(0.79874874277943,0.601664728821858,0.));
#6661=DIRECTION('',(0.,0.,-1.));
#6662=DIRECTION('center_axis',(0.,0.,-1.));
#6663=DIRECTION('ref_axis',(0.894892375881552,-0.446282013517317,0.));
#6664=DIRECTION('',(0.,0.,1.));
#6665=DIRECTION('center_axis',(0.,0.,1.));
#6666=DIRECTION('ref_axis',(-1.,1.22464679914735E-16,0.));
#6667=DIRECTION('center_axis',(-0.601664728821861,-0.798748742779428,3.54715698049647E-15));
#6668=DIRECTION('ref_axis',(0.798748742779428,-0.601664728821861,-1.85390118736899E-31));
#6669=DIRECTION('center_axis',(0.,0.,1.));
#6670=DIRECTION('ref_axis',(-1.,1.22464679914735E-16,0.));
#6671=DIRECTION('center_axis',(-0.601664728821861,0.798748742779428,3.54715698049647E-15));
#6672=DIRECTION('ref_axis',(-2.50378775993336E-30,-4.44089209850063E-15,
1.));
#6673=DIRECTION('center_axis',(0.,0.,-1.));
#6674=DIRECTION('ref_axis',(-1.,1.22464679914735E-16,0.));
#6675=DIRECTION('center_axis',(-0.185467508428577,-0.954822547310801,-0.232197559126295));
#6676=DIRECTION('ref_axis',(0.595903538017452,-0.297176552148574,0.746046292284446));
#6677=DIRECTION('center_axis',(1.,0.,0.));
#6678=DIRECTION('ref_axis',(0.,-0.707106781186546,0.707106781186549));
#6679=DIRECTION('center_axis',(0.,0.,-1.));
#6680=DIRECTION('ref_axis',(0.894892375881552,0.446282013517317,0.));
#6681=DIRECTION('center_axis',(0.,0.,-1.));
#6682=DIRECTION('ref_axis',(0.,1.,0.));
#6683=DIRECTION('',(0.,0.,-1.));
#6684=DIRECTION('center_axis',(0.,0.,-1.));
#6685=DIRECTION('ref_axis',(0.894892375881552,0.446282013517317,0.));
#6686=DIRECTION('',(0.,0.,1.));
#6687=DIRECTION('center_axis',(0.185467508428577,-0.954822547310802,0.23219755912629));
#6688=DIRECTION('ref_axis',(0.595903538017456,0.297176552148567,0.746046292284445));
#6689=DIRECTION('center_axis',(1.,0.,0.));
#6690=DIRECTION('ref_axis',(0.,0.707106781186546,0.707106781186549));
#6691=DIRECTION('center_axis',(0.,-1.,0.));
#6692=DIRECTION('ref_axis',(-1.,0.,0.));
#6693=DIRECTION('',(-1.,0.,0.));
#6694=DIRECTION('',(1.,0.,0.));
#6695=DIRECTION('',(0.,0.,1.));
#6696=DIRECTION('',(-1.,0.,0.));
#6697=DIRECTION('center_axis',(-1.,0.,0.));
#6698=DIRECTION('ref_axis',(0.,-0.707106781186547,0.707106781186548));
#6699=DIRECTION('',(-1.,0.,0.));
#6700=DIRECTION('center_axis',(1.,0.,0.));
#6701=DIRECTION('ref_axis',(0.,0.,1.));
#6702=DIRECTION('center_axis',(0.,0.,1.));
#6703=DIRECTION('ref_axis',(1.,0.,0.));
#6704=DIRECTION('',(1.,0.,0.));
#6705=DIRECTION('center_axis',(0.,0.,-1.));
#6706=DIRECTION('ref_axis',(-0.707106781186548,0.707106781186547,0.));
#6707=DIRECTION('',(0.,1.,0.));
#6708=DIRECTION('center_axis',(0.,0.,-1.));
#6709=DIRECTION('ref_axis',(-0.707106781186548,-0.707106781186547,0.));
#6710=DIRECTION('center_axis',(0.,0.,1.));
#6711=DIRECTION('ref_axis',(1.,0.,0.));
#6712=DIRECTION('center_axis',(1.,0.,0.));
#6713=DIRECTION('ref_axis',(0.,0.707106781186547,0.707106781186548));
#6714=DIRECTION('',(-1.,0.,0.));
#6715=DIRECTION('center_axis',(-1.,0.,0.));
#6716=DIRECTION('ref_axis',(0.,0.,1.));
#6717=DIRECTION('center_axis',(0.,1.,0.));
#6718=DIRECTION('ref_axis',(1.,0.,0.));
#6719=DIRECTION('',(1.,0.,0.));
#6720=DIRECTION('',(1.,0.,0.));
#6721=DIRECTION('',(0.,0.,-1.));
#6722=DIRECTION('center_axis',(0.,0.,-1.));
#6723=DIRECTION('ref_axis',(-1.,0.,0.));
#6724=DIRECTION('center_axis',(2.22044604925032E-15,-1.,0.));
#6725=DIRECTION('ref_axis',(0.,0.,1.));
#6726=DIRECTION('center_axis',(0.,0.,1.));
#6727=DIRECTION('ref_axis',(-0.707106781186548,-0.707106781186547,0.));
#6728=DIRECTION('center_axis',(0.,1.,0.));
#6729=DIRECTION('ref_axis',(-0.707106781186547,0.,0.707106781186548));
#6730=DIRECTION('center_axis',(-2.22044604925032E-15,-1.,0.));
#6731=DIRECTION('ref_axis',(0.,0.,1.));
#6732=DIRECTION('',(0.,-1.,0.));
#6733=DIRECTION('center_axis',(0.,0.,-1.));
#6734=DIRECTION('ref_axis',(-1.,0.,0.));
#6735=DIRECTION('center_axis',(0.,0.,1.));
#6736=DIRECTION('ref_axis',(-0.707106781186548,0.707106781186547,0.));
#6737=DIRECTION('center_axis',(0.,0.,1.));
#6738=DIRECTION('ref_axis',(1.,0.,0.));
#6739=DIRECTION('center_axis',(0.,0.,-1.));
#6740=DIRECTION('ref_axis',(1.,0.,0.));
#6741=DIRECTION('',(-0.707106781186548,-8.65956056235494E-17,0.707106781186547));
#6742=DIRECTION('center_axis',(0.,0.,-1.));
#6743=DIRECTION('ref_axis',(1.,0.,0.));
#6744=DIRECTION('',(0.,0.,-1.));
#6745=DIRECTION('center_axis',(0.,0.,1.));
#6746=DIRECTION('ref_axis',(1.,0.,0.));
#6747=DIRECTION('center_axis',(0.,0.,-1.));
#6748=DIRECTION('ref_axis',(-0.707106781186548,-0.707106781186548,0.));
#6749=DIRECTION('',(0.,0.,-1.));
#6750=DIRECTION('center_axis',(0.,0.,1.));
#6751=DIRECTION('ref_axis',(-0.707106781186548,-0.707106781186548,0.));
#6752=DIRECTION('center_axis',(-1.,0.,0.));
#6753=DIRECTION('ref_axis',(0.,1.,0.));
#6754=DIRECTION('',(0.,0.,1.));
#6755=DIRECTION('',(0.,1.,0.));
#6756=DIRECTION('center_axis',(0.,0.,-1.));
#6757=DIRECTION('ref_axis',(-0.707106781186548,0.707106781186548,0.));
#6758=DIRECTION('center_axis',(0.,0.,1.));
#6759=DIRECTION('ref_axis',(-0.707106781186548,0.707106781186548,0.));
#6760=DIRECTION('center_axis',(0.,0.,-1.));
#6761=DIRECTION('ref_axis',(-1.,-1.22464679914735E-16,0.));
#6762=DIRECTION('center_axis',(0.,0.,-1.));
#6763=DIRECTION('ref_axis',(1.,0.,0.));
#6764=DIRECTION('center_axis',(0.,0.,1.));
#6765=DIRECTION('ref_axis',(1.,0.,0.));
#6766=DIRECTION('center_axis',(0.,0.,1.));
#6767=DIRECTION('ref_axis',(1.,0.,0.));
#6768=DIRECTION('',(0.,0.,1.));
#6769=DIRECTION('center_axis',(0.,0.,1.));
#6770=DIRECTION('ref_axis',(1.,0.,0.));
#6771=DIRECTION('center_axis',(0.,0.,1.));
#6772=DIRECTION('ref_axis',(1.,0.,0.));
#6773=DIRECTION('center_axis',(0.,0.,-1.));
#6774=DIRECTION('ref_axis',(-1.,0.,0.));
#6775=DIRECTION('center_axis',(0.,0.,1.));
#6776=DIRECTION('ref_axis',(1.,0.,0.));
#6777=DIRECTION('center_axis',(0.,0.,1.));
#6778=DIRECTION('ref_axis',(1.,0.,0.));
#6779=DIRECTION('center_axis',(0.,0.,1.));
#6780=DIRECTION('ref_axis',(1.,0.,0.));
#6781=DIRECTION('center_axis',(0.,0.,1.));
#6782=DIRECTION('ref_axis',(1.,0.,0.));
#6783=DIRECTION('',(0.,0.,-1.));
#6784=DIRECTION('center_axis',(0.,0.,1.));
#6785=DIRECTION('ref_axis',(1.,0.,0.));
#6786=DIRECTION('center_axis',(0.,0.,1.));
#6787=DIRECTION('ref_axis',(1.,0.,0.));
#6788=DIRECTION('center_axis',(0.,0.,1.));
#6789=DIRECTION('ref_axis',(1.,0.,0.));
#6790=DIRECTION('center_axis',(0.,0.,1.));
#6791=DIRECTION('ref_axis',(1.,0.,0.));
#6792=DIRECTION('',(0.,0.,-1.));
#6793=DIRECTION('center_axis',(0.,0.,1.));
#6794=DIRECTION('ref_axis',(1.,0.,0.));
#6795=DIRECTION('axis',(0.,0.,1.));
#6796=DIRECTION('refdir',(1.,0.,0.));
#6797=DIRECTION('center_axis',(0.,0.,1.));
#6798=DIRECTION('ref_axis',(1.,0.,0.));
#6799=DIRECTION('center_axis',(1.22464679914735E-16,-1.,0.));
#6800=DIRECTION('ref_axis',(-1.,-1.22464679914735E-16,0.));
#6801=DIRECTION('center_axis',(0.,0.,-1.));
#6802=DIRECTION('ref_axis',(1.,0.,0.));
#6803=DIRECTION('',(0.,0.,1.));
#6804=DIRECTION('',(1.,0.,0.));
#6805=DIRECTION('',(0.,0.,1.));
#6806=DIRECTION('',(1.,0.,0.));
#6807=DIRECTION('',(0.,0.,1.));
#6808=DIRECTION('',(1.,0.,0.));
#6809=DIRECTION('',(0.,0.,1.));
#6810=DIRECTION('',(1.,0.,0.));
#6811=DIRECTION('',(0.,0.,1.));
#6812=DIRECTION('',(1.,0.,0.));
#6813=DIRECTION('',(0.,0.,1.));
#6814=DIRECTION('',(1.,0.,0.));
#6815=DIRECTION('',(0.,0.,1.));
#6816=DIRECTION('',(1.,0.,0.));
#6817=CARTESIAN_POINT('',(0.,0.,0.));
#6818=CARTESIAN_POINT('',(0.,0.,0.));
#6819=CARTESIAN_POINT('Origin',(0.,0.,13.));
#6820=CARTESIAN_POINT('',(5.,6.12323399573677E-16,13.));
#6821=CARTESIAN_POINT('Origin',(0.,0.,13.));
#6822=CARTESIAN_POINT('',(5.,6.12323399573677E-16,0.));
#6823=CARTESIAN_POINT('',(5.,-6.12323399573677E-16,13.));
#6824=CARTESIAN_POINT('Origin',(0.,0.,0.));
#6825=CARTESIAN_POINT('Origin',(18.4254989505611,-3.10927393821618,0.));
#6826=CARTESIAN_POINT('',(17.4394399250575,-2.94287803014511,13.));
#6827=CARTESIAN_POINT('',(18.2065715530743,-4.08501508966447,13.));
#6828=CARTESIAN_POINT('Origin',(18.4254989505611,-3.10927393821618,13.));
#6829=CARTESIAN_POINT('',(18.2065715530743,-4.08501508966447,0.));
#6830=CARTESIAN_POINT('',(18.2065715530743,-4.08501508966447,0.));
#6831=CARTESIAN_POINT('',(17.4394399250575,-2.94287803014511,0.));
#6832=CARTESIAN_POINT('Origin',(18.4254989505611,-3.10927393821618,0.));
#6833=CARTESIAN_POINT('',(17.4394399250575,-2.94287803014511,0.));
#6834=CARTESIAN_POINT('Origin',(18.337935196262,-4.11448919812531,0.));
#6835=CARTESIAN_POINT('',(18.337935196262,-4.11448919812531,13.));
#6836=CARTESIAN_POINT('',(9.16896759813102,-2.05724459906266,13.));
#6837=CARTESIAN_POINT('',(18.337935196262,-4.11448919812531,0.));
#6838=CARTESIAN_POINT('',(18.337935196262,-4.11448919812531,0.));
#6839=CARTESIAN_POINT('',(17.2472005929999,-3.86976067797773,0.));
#6840=CARTESIAN_POINT('Origin',(16.7341271470625,-8.31478109308627,0.));
#6841=CARTESIAN_POINT('',(15.8385835771673,-7.8698072574293,0.));
#6842=CARTESIAN_POINT('',(17.1305374208376,-7.39670762388808,0.));
#6843=CARTESIAN_POINT('Origin',(16.7341271470625,-8.31478109308627,0.));
#6844=CARTESIAN_POINT('',(17.1305374208376,-7.39670762388808,13.));
#6845=CARTESIAN_POINT('',(17.1305374208376,-7.39670762388808,0.));
#6846=CARTESIAN_POINT('',(15.8385835771673,-7.8698072574293,13.));
#6847=CARTESIAN_POINT('Origin',(16.7341271470625,-8.31478109308627,13.));
#6848=CARTESIAN_POINT('',(15.8385835771673,-7.8698072574293,0.));
#6849=CARTESIAN_POINT('Origin',(16.2278666415473,-7.00694799924747,0.));
#6850=CARTESIAN_POINT('',(17.2541372868972,-7.45007618140239,0.));
#6851=CARTESIAN_POINT('',(16.2278666415473,-7.00694799924747,0.));
#6852=CARTESIAN_POINT('',(17.2541372868972,-7.45007618140239,13.));
#6853=CARTESIAN_POINT('',(17.2541372868972,-7.45007618140239,0.));
#6854=CARTESIAN_POINT('',(8.11393332077363,-3.50347399962373,13.));
#6855=CARTESIAN_POINT('Origin',(16.5628723558448,-8.65088754544835,0.));
#6856=CARTESIAN_POINT('',(15.6764936575763,-8.18792663645507,13.));
#6857=CARTESIAN_POINT('',(16.0531394299608,-9.51122023939286,13.));
#6858=CARTESIAN_POINT('Origin',(16.5628723558448,-8.65088754544835,13.));
#6859=CARTESIAN_POINT('',(16.0531394299608,-9.51122023939286,0.));
#6860=CARTESIAN_POINT('',(16.0531394299608,-9.51122023939286,0.));
#6861=CARTESIAN_POINT('',(15.6764936575763,-8.18792663645507,0.));
#6862=CARTESIAN_POINT('Origin',(16.5628723558448,-8.65088754544835,0.));
#6863=CARTESIAN_POINT('',(15.6764936575763,-8.18792663645507,0.));
#6864=CARTESIAN_POINT('Origin',(16.1689656784104,-9.57984538049455,0.));
#6865=CARTESIAN_POINT('',(16.1689656784104,-9.57984538049455,13.));
#6866=CARTESIAN_POINT('',(8.08448283920519,-4.78992269024728,13.));
#6867=CARTESIAN_POINT('',(16.1689656784104,-9.57984538049455,0.));
#6868=CARTESIAN_POINT('',(16.1689656784104,-9.57984538049455,0.));
#6869=CARTESIAN_POINT('',(15.2072406981632,-9.01003919792413,0.));
#6870=CARTESIAN_POINT('Origin',(13.3456920054543,-13.0789564146209,0.));
#6871=CARTESIAN_POINT('',(12.6314839349494,-12.3790229663377,0.));
#6872=CARTESIAN_POINT('',(14.0064008835214,-12.3283141706436,0.));
#6873=CARTESIAN_POINT('Origin',(13.3456920054543,-13.0789564146209,0.));
#6874=CARTESIAN_POINT('',(14.0064008835214,-12.3283141706436,13.));
#6875=CARTESIAN_POINT('',(14.0064008835214,-12.3283141706436,0.));
#6876=CARTESIAN_POINT('',(12.6314839349494,-12.3790229663377,13.));
#6877=CARTESIAN_POINT('Origin',(13.3456920054543,-13.0789564146209,13.));
#6878=CARTESIAN_POINT('',(12.6314839349494,-12.3790229663377,0.));
#6879=CARTESIAN_POINT('Origin',(13.2683523045433,-11.678690128714,0.));
#6880=CARTESIAN_POINT('',(14.1074595503134,-12.4172651441477,0.));
#6881=CARTESIAN_POINT('',(13.2683523045433,-11.678690128714,0.));
#6882=CARTESIAN_POINT('',(14.1074595503134,-12.4172651441477,13.));
#6883=CARTESIAN_POINT('',(14.1074595503134,-12.4172651441477,0.));
#6884=CARTESIAN_POINT('',(6.63417615227163,-5.839345064357,13.));
#6885=CARTESIAN_POINT('Origin',(13.0789564146209,-13.3456920054543,0.));
#6886=CARTESIAN_POINT('',(12.3790229663377,-12.6314839349494,13.));
#6887=CARTESIAN_POINT('',(12.3283141706436,-14.0064008835214,13.));
#6888=CARTESIAN_POINT('Origin',(13.0789564146209,-13.3456920054543,13.));
#6889=CARTESIAN_POINT('',(12.3283141706436,-14.0064008835214,0.));
#6890=CARTESIAN_POINT('',(12.3283141706436,-14.0064008835214,0.));
#6891=CARTESIAN_POINT('',(12.3790229663377,-12.6314839349494,0.));
#6892=CARTESIAN_POINT('Origin',(13.0789564146209,-13.3456920054543,0.));
#6893=CARTESIAN_POINT('',(12.3790229663377,-12.6314839349494,0.));
#6894=CARTESIAN_POINT('Origin',(12.4172651441477,-14.1074595503134,0.));
#6895=CARTESIAN_POINT('',(12.4172651441477,-14.1074595503134,13.));
#6896=CARTESIAN_POINT('',(6.20863257207386,-7.05372977515671,13.));
#6897=CARTESIAN_POINT('',(12.4172651441477,-14.1074595503134,0.));
#6898=CARTESIAN_POINT('',(12.4172651441477,-14.1074595503134,0.));
#6899=CARTESIAN_POINT('',(11.678690128714,-13.2683523045433,0.));
#6900=CARTESIAN_POINT('Origin',(8.65088754544834,-16.5628723558448,0.));
#6901=CARTESIAN_POINT('',(8.18792663645507,-15.6764936575763,0.));
#6902=CARTESIAN_POINT('',(9.51122023939285,-16.0531394299608,0.));
#6903=CARTESIAN_POINT('Origin',(8.65088754544834,-16.5628723558448,0.));
#6904=CARTESIAN_POINT('',(9.51122023939285,-16.0531394299608,13.));
#6905=CARTESIAN_POINT('',(9.51122023939285,-16.0531394299608,0.));
#6906=CARTESIAN_POINT('',(8.18792663645507,-15.6764936575763,13.));
#6907=CARTESIAN_POINT('Origin',(8.65088754544834,-16.5628723558448,13.));
#6908=CARTESIAN_POINT('',(8.18792663645507,-15.6764936575763,0.));
#6909=CARTESIAN_POINT('Origin',(9.01003919792412,-15.2072406981632,0.));
#6910=CARTESIAN_POINT('',(9.57984538049454,-16.1689656784104,0.));
#6911=CARTESIAN_POINT('',(9.01003919792412,-15.2072406981632,0.));
#6912=CARTESIAN_POINT('',(9.57984538049454,-16.1689656784104,13.));
#6913=CARTESIAN_POINT('',(9.57984538049454,-16.1689656784104,0.));
#6914=CARTESIAN_POINT('',(4.50501959896206,-7.6036203490816,13.));
#6915=CARTESIAN_POINT('Origin',(8.31478109308627,-16.7341271470625,0.));
#6916=CARTESIAN_POINT('',(7.86980725742929,-15.8385835771673,13.));
#6917=CARTESIAN_POINT('',(7.39670762388807,-17.1305374208376,13.));
#6918=CARTESIAN_POINT('Origin',(8.31478109308627,-16.7341271470625,13.));
#6919=CARTESIAN_POINT('',(7.39670762388807,-17.1305374208376,0.));
#6920=CARTESIAN_POINT('',(7.39670762388807,-17.1305374208376,0.));
#6921=CARTESIAN_POINT('',(7.86980725742929,-15.8385835771673,0.));
#6922=CARTESIAN_POINT('Origin',(8.31478109308627,-16.7341271470625,0.));
#6923=CARTESIAN_POINT('',(7.86980725742929,-15.8385835771673,0.));
#6924=CARTESIAN_POINT('Origin',(7.45007618140238,-17.2541372868972,0.));
#6925=CARTESIAN_POINT('',(7.45007618140238,-17.2541372868972,13.));
#6926=CARTESIAN_POINT('',(3.72503809070119,-8.62706864344861,13.));
#6927=CARTESIAN_POINT('',(7.45007618140238,-17.2541372868972,0.));
#6928=CARTESIAN_POINT('',(7.45007618140238,-17.2541372868972,0.));
#6929=CARTESIAN_POINT('',(7.00694799924746,-16.2278666415473,0.));
#6930=CARTESIAN_POINT('Origin',(3.10927393821617,-18.4254989505611,0.));
#6931=CARTESIAN_POINT('',(2.9428780301451,-17.4394399250575,0.));
#6932=CARTESIAN_POINT('',(4.08501508966446,-18.2065715530743,0.));
#6933=CARTESIAN_POINT('Origin',(3.10927393821617,-18.4254989505611,0.));
#6934=CARTESIAN_POINT('',(4.08501508966446,-18.2065715530743,13.));
#6935=CARTESIAN_POINT('',(4.08501508966446,-18.2065715530743,0.));
#6936=CARTESIAN_POINT('',(2.9428780301451,-17.4394399250575,13.));
#6937=CARTESIAN_POINT('Origin',(3.10927393821617,-18.4254989505611,13.));
#6938=CARTESIAN_POINT('',(2.9428780301451,-17.4394399250575,0.));
#6939=CARTESIAN_POINT('Origin',(3.86976067797772,-17.2472005929999,0.));
#6940=CARTESIAN_POINT('',(4.1144891981253,-18.337935196262,0.));
#6941=CARTESIAN_POINT('',(3.86976067797772,-17.2472005929999,0.));
#6942=CARTESIAN_POINT('',(4.1144891981253,-18.337935196262,13.));
#6943=CARTESIAN_POINT('',(4.1144891981253,-18.337935196262,0.));
#6944=CARTESIAN_POINT('',(1.93488033898886,-8.62360029649997,13.));
#6945=CARTESIAN_POINT('Origin',(2.73669706567396,-18.4845093299966,0.));
#6946=CARTESIAN_POINT('',(2.59023998199238,-17.4952923049513,13.));
#6947=CARTESIAN_POINT('',(1.741059799014,-18.5778175999297,13.));
#6948=CARTESIAN_POINT('Origin',(2.73669706567396,-18.4845093299966,13.));
#6949=CARTESIAN_POINT('',(1.741059799014,-18.5778175999297,0.));
#6950=CARTESIAN_POINT('',(1.741059799014,-18.5778175999297,0.));
#6951=CARTESIAN_POINT('',(2.59023998199238,-17.4952923049513,0.));
#6952=CARTESIAN_POINT('Origin',(2.73669706567396,-18.4845093299966,0.));
#6953=CARTESIAN_POINT('',(2.59023998199238,-17.4952923049513,0.));
#6954=CARTESIAN_POINT('Origin',(1.75362185428836,-18.7118598491961,0.));
#6955=CARTESIAN_POINT('',(1.75362185428836,-18.7118598491961,13.));
#6956=CARTESIAN_POINT('',(0.876810927144179,-9.35592992459806,13.));
#6957=CARTESIAN_POINT('',(1.75362185428836,-18.7118598491961,0.));
#6958=CARTESIAN_POINT('',(1.75362185428836,-18.7118598491961,0.));
#6959=CARTESIAN_POINT('',(1.64931697933718,-17.5988843254813,0.));
#6960=CARTESIAN_POINT('Origin',(-2.73669706567396,-18.4845093299966,0.));
#6961=CARTESIAN_POINT('',(-2.59023998199239,-17.4952923049513,0.));
#6962=CARTESIAN_POINT('',(-1.74105979901401,-18.5778175999297,0.));
#6963=CARTESIAN_POINT('Origin',(-2.73669706567396,-18.4845093299966,0.));
#6964=CARTESIAN_POINT('',(-1.74105979901401,-18.5778175999297,13.));
#6965=CARTESIAN_POINT('',(-1.74105979901401,-18.5778175999297,0.));
#6966=CARTESIAN_POINT('',(-2.59023998199239,-17.4952923049513,13.));
#6967=CARTESIAN_POINT('Origin',(-2.73669706567396,-18.4845093299966,13.));
#6968=CARTESIAN_POINT('',(-2.59023998199239,-17.4952923049513,0.));
#6969=CARTESIAN_POINT('Origin',(-1.64931697933719,-17.5988843254813,0.));
#6970=CARTESIAN_POINT('',(-1.75362185428837,-18.7118598491961,0.));
#6971=CARTESIAN_POINT('',(-1.64931697933719,-17.5988843254813,0.));
#6972=CARTESIAN_POINT('',(-1.75362185428837,-18.7118598491961,13.));
#6973=CARTESIAN_POINT('',(-1.75362185428837,-18.7118598491961,0.));
#6974=CARTESIAN_POINT('',(-0.824658489668592,-8.79944216274063,13.));
#6975=CARTESIAN_POINT('Origin',(-3.10927393821618,-18.4254989505611,0.));
#6976=CARTESIAN_POINT('',(-2.94287803014511,-17.4394399250575,13.));
#6977=CARTESIAN_POINT('',(-4.08501508966447,-18.2065715530743,13.));
#6978=CARTESIAN_POINT('Origin',(-3.10927393821618,-18.4254989505611,13.));
#6979=CARTESIAN_POINT('',(-4.08501508966447,-18.2065715530743,0.));
#6980=CARTESIAN_POINT('',(-4.08501508966447,-18.2065715530743,0.));
#6981=CARTESIAN_POINT('',(-2.94287803014511,-17.4394399250575,0.));
#6982=CARTESIAN_POINT('Origin',(-3.10927393821618,-18.4254989505611,0.));
#6983=CARTESIAN_POINT('',(-2.94287803014511,-17.4394399250575,0.));
#6984=CARTESIAN_POINT('Origin',(-4.11448919812531,-18.337935196262,0.));
#6985=CARTESIAN_POINT('',(-4.11448919812531,-18.337935196262,13.));
#6986=CARTESIAN_POINT('',(-2.05724459906266,-9.16896759813102,13.));
#6987=CARTESIAN_POINT('',(-4.11448919812531,-18.337935196262,0.));
#6988=CARTESIAN_POINT('',(-4.11448919812531,-18.337935196262,0.));
#6989=CARTESIAN_POINT('',(-3.86976067797773,-17.2472005929999,0.));
#6990=CARTESIAN_POINT('Origin',(-8.31478109308627,-16.7341271470625,0.));
#6991=CARTESIAN_POINT('',(-7.86980725742929,-15.8385835771673,0.));
#6992=CARTESIAN_POINT('',(-7.39670762388808,-17.1305374208376,0.));
#6993=CARTESIAN_POINT('Origin',(-8.31478109308627,-16.7341271470625,0.));
#6994=CARTESIAN_POINT('',(-7.39670762388808,-17.1305374208376,13.));
#6995=CARTESIAN_POINT('',(-7.39670762388808,-17.1305374208376,0.));
#6996=CARTESIAN_POINT('',(-7.86980725742929,-15.8385835771673,13.));
#6997=CARTESIAN_POINT('Origin',(-8.31478109308627,-16.7341271470625,13.));
#6998=CARTESIAN_POINT('',(-7.86980725742929,-15.8385835771673,0.));
#6999=CARTESIAN_POINT('Origin',(-7.00694799924747,-16.2278666415473,0.));
#7000=CARTESIAN_POINT('',(-7.45007618140239,-17.2541372868972,0.));
#7001=CARTESIAN_POINT('',(-7.00694799924747,-16.2278666415473,0.));
#7002=CARTESIAN_POINT('',(-7.45007618140239,-17.2541372868972,13.));
#7003=CARTESIAN_POINT('',(-7.45007618140239,-17.2541372868972,0.));
#7004=CARTESIAN_POINT('',(-3.50347399962373,-8.11393332077363,13.));
#7005=CARTESIAN_POINT('Origin',(-8.65088754544835,-16.5628723558448,0.));
#7006=CARTESIAN_POINT('',(-8.18792663645507,-15.6764936575763,13.));
#7007=CARTESIAN_POINT('',(-9.51122023939286,-16.0531394299608,13.));
#7008=CARTESIAN_POINT('Origin',(-8.65088754544835,-16.5628723558448,13.));
#7009=CARTESIAN_POINT('',(-9.51122023939286,-16.0531394299608,0.));
#7010=CARTESIAN_POINT('',(-9.51122023939286,-16.0531394299608,0.));
#7011=CARTESIAN_POINT('',(-8.18792663645507,-15.6764936575763,0.));
#7012=CARTESIAN_POINT('Origin',(-8.65088754544835,-16.5628723558448,0.));
#7013=CARTESIAN_POINT('',(-8.18792663645507,-15.6764936575763,0.));
#7014=CARTESIAN_POINT('Origin',(-9.57984538049455,-16.1689656784104,0.));
#7015=CARTESIAN_POINT('',(-9.57984538049455,-16.1689656784104,13.));
#7016=CARTESIAN_POINT('',(-4.78992269024728,-8.08448283920519,13.));
#7017=CARTESIAN_POINT('',(-9.57984538049455,-16.1689656784104,0.));
#7018=CARTESIAN_POINT('',(-9.57984538049455,-16.1689656784104,0.));
#7019=CARTESIAN_POINT('',(-9.01003919792412,-15.2072406981632,0.));
#7020=CARTESIAN_POINT('Origin',(-13.0789564146209,-13.3456920054543,0.));
#7021=CARTESIAN_POINT('',(-12.3790229663377,-12.6314839349494,0.));
#7022=CARTESIAN_POINT('',(-12.3283141706436,-14.0064008835214,0.));
#7023=CARTESIAN_POINT('Origin',(-13.0789564146209,-13.3456920054543,0.));
#7024=CARTESIAN_POINT('',(-12.3283141706436,-14.0064008835214,13.));
#7025=CARTESIAN_POINT('',(-12.3283141706436,-14.0064008835214,0.));
#7026=CARTESIAN_POINT('',(-12.3790229663377,-12.6314839349494,13.));
#7027=CARTESIAN_POINT('Origin',(-13.0789564146209,-13.3456920054543,13.));
#7028=CARTESIAN_POINT('',(-12.3790229663377,-12.6314839349494,0.));
#7029=CARTESIAN_POINT('Origin',(-11.678690128714,-13.2683523045433,0.));
#7030=CARTESIAN_POINT('',(-12.4172651441477,-14.1074595503134,0.));
#7031=CARTESIAN_POINT('',(-11.678690128714,-13.2683523045433,0.));
#7032=CARTESIAN_POINT('',(-12.4172651441477,-14.1074595503134,13.));
#7033=CARTESIAN_POINT('',(-12.4172651441477,-14.1074595503134,0.));
#7034=CARTESIAN_POINT('',(-5.83934506435699,-6.63417615227163,13.));
#7035=CARTESIAN_POINT('Origin',(-13.3456920054543,-13.0789564146209,0.));
#7036=CARTESIAN_POINT('',(-12.6314839349494,-12.3790229663377,13.));
#7037=CARTESIAN_POINT('',(-14.0064008835214,-12.3283141706436,13.));
#7038=CARTESIAN_POINT('Origin',(-13.3456920054543,-13.0789564146209,13.));
#7039=CARTESIAN_POINT('',(-14.0064008835214,-12.3283141706436,0.));
#7040=CARTESIAN_POINT('',(-14.0064008835214,-12.3283141706436,0.));
#7041=CARTESIAN_POINT('',(-12.6314839349494,-12.3790229663377,0.));
#7042=CARTESIAN_POINT('Origin',(-13.3456920054543,-13.0789564146209,0.));
#7043=CARTESIAN_POINT('',(-12.6314839349494,-12.3790229663377,0.));
#7044=CARTESIAN_POINT('Origin',(-14.1074595503134,-12.4172651441477,0.));
#7045=CARTESIAN_POINT('',(-14.1074595503134,-12.4172651441477,13.));
#7046=CARTESIAN_POINT('',(-7.05372977515671,-6.20863257207387,13.));
#7047=CARTESIAN_POINT('',(-14.1074595503134,-12.4172651441477,0.));
#7048=CARTESIAN_POINT('',(-14.1074595503134,-12.4172651441477,0.));
#7049=CARTESIAN_POINT('',(-13.2683523045433,-11.678690128714,0.));
#7050=CARTESIAN_POINT('Origin',(-16.5628723558448,-8.65088754544834,0.));
#7051=CARTESIAN_POINT('',(-15.6764936575763,-8.18792663645507,0.));
#7052=CARTESIAN_POINT('',(-16.0531394299608,-9.51122023939286,0.));
#7053=CARTESIAN_POINT('Origin',(-16.5628723558448,-8.65088754544834,0.));
#7054=CARTESIAN_POINT('',(-16.0531394299608,-9.51122023939286,13.));
#7055=CARTESIAN_POINT('',(-16.0531394299608,-9.51122023939286,0.));
#7056=CARTESIAN_POINT('',(-15.6764936575763,-8.18792663645507,13.));
#7057=CARTESIAN_POINT('Origin',(-16.5628723558448,-8.65088754544834,13.));
#7058=CARTESIAN_POINT('',(-15.6764936575763,-8.18792663645507,0.));
#7059=CARTESIAN_POINT('Origin',(-15.2072406981632,-9.01003919792412,0.));
#7060=CARTESIAN_POINT('',(-16.1689656784104,-9.57984538049455,0.));
#7061=CARTESIAN_POINT('',(-15.2072406981632,-9.01003919792412,0.));
#7062=CARTESIAN_POINT('',(-16.1689656784104,-9.57984538049455,13.));
#7063=CARTESIAN_POINT('',(-16.1689656784104,-9.57984538049455,0.));
#7064=CARTESIAN_POINT('',(-7.6036203490816,-4.50501959896206,13.));
#7065=CARTESIAN_POINT('Origin',(-16.7341271470625,-8.31478109308626,0.));
#7066=CARTESIAN_POINT('',(-15.8385835771673,-7.86980725742929,13.));
#7067=CARTESIAN_POINT('',(-17.1305374208376,-7.39670762388807,13.));
#7068=CARTESIAN_POINT('Origin',(-16.7341271470625,-8.31478109308626,13.));
#7069=CARTESIAN_POINT('',(-17.1305374208376,-7.39670762388807,0.));
#7070=CARTESIAN_POINT('',(-17.1305374208376,-7.39670762388807,0.));
#7071=CARTESIAN_POINT('',(-15.8385835771673,-7.86980725742929,0.));
#7072=CARTESIAN_POINT('Origin',(-16.7341271470625,-8.31478109308626,0.));
#7073=CARTESIAN_POINT('',(-15.8385835771673,-7.86980725742929,0.));
#7074=CARTESIAN_POINT('Origin',(-17.2541372868972,-7.45007618140238,0.));
#7075=CARTESIAN_POINT('',(-17.2541372868972,-7.45007618140238,13.));
#7076=CARTESIAN_POINT('',(-8.62706864344861,-3.72503809070119,13.));
#7077=CARTESIAN_POINT('',(-17.2541372868972,-7.45007618140238,0.));
#7078=CARTESIAN_POINT('',(-17.2541372868972,-7.45007618140238,0.));
#7079=CARTESIAN_POINT('',(-16.2278666415473,-7.00694799924746,0.));
#7080=CARTESIAN_POINT('Origin',(-18.4254989505611,-3.10927393821617,0.));
#7081=CARTESIAN_POINT('',(-17.4394399250575,-2.94287803014509,0.));
#7082=CARTESIAN_POINT('',(-18.2065715530743,-4.08501508966446,0.));
#7083=CARTESIAN_POINT('Origin',(-18.4254989505611,-3.10927393821617,0.));
#7084=CARTESIAN_POINT('',(-18.2065715530743,-4.08501508966447,13.));
#7085=CARTESIAN_POINT('',(-18.2065715530743,-4.08501508966447,0.));
#7086=CARTESIAN_POINT('',(-17.4394399250575,-2.94287803014509,13.));
#7087=CARTESIAN_POINT('Origin',(-18.4254989505611,-3.10927393821617,13.));
#7088=CARTESIAN_POINT('',(-17.4394399250575,-2.94287803014509,0.));
#7089=CARTESIAN_POINT('Origin',(-17.2472005929999,-3.86976067797772,0.));
#7090=CARTESIAN_POINT('',(-18.337935196262,-4.1144891981253,0.));
#7091=CARTESIAN_POINT('',(-17.2472005929999,-3.86976067797772,0.));
#7092=CARTESIAN_POINT('',(-18.337935196262,-4.1144891981253,13.));
#7093=CARTESIAN_POINT('',(-18.337935196262,-4.1144891981253,0.));
#7094=CARTESIAN_POINT('',(-8.62360029649997,-1.93488033898886,13.));
#7095=CARTESIAN_POINT('Origin',(-18.4845093299966,-2.73669706567395,0.));
#7096=CARTESIAN_POINT('',(-17.4952923049513,-2.59023998199238,13.));
#7097=CARTESIAN_POINT('',(-18.5778175999297,-1.74105979901401,13.));
#7098=CARTESIAN_POINT('Origin',(-18.4845093299966,-2.73669706567395,13.));
#7099=CARTESIAN_POINT('',(-18.5778175999297,-1.74105979901401,0.));
#7100=CARTESIAN_POINT('',(-18.5778175999297,-1.74105979901401,0.));
#7101=CARTESIAN_POINT('',(-17.4952923049513,-2.59023998199238,0.));
#7102=CARTESIAN_POINT('Origin',(-18.4845093299966,-2.73669706567395,0.));
#7103=CARTESIAN_POINT('',(-17.4952923049513,-2.59023998199238,0.));
#7104=CARTESIAN_POINT('Origin',(-18.7118598491961,-1.75362185428836,0.));
#7105=CARTESIAN_POINT('',(-18.7118598491961,-1.75362185428836,13.));
#7106=CARTESIAN_POINT('',(-9.35592992459806,-0.87681092714418,13.));
#7107=CARTESIAN_POINT('',(-18.7118598491961,-1.75362185428836,0.));
#7108=CARTESIAN_POINT('',(-18.7118598491961,-1.75362185428836,0.));
#7109=CARTESIAN_POINT('',(-17.5988843254813,-1.64931697933718,0.));
#7110=CARTESIAN_POINT('Origin',(-18.4845093299966,2.73669706567396,0.));
#7111=CARTESIAN_POINT('',(-17.4952923049513,2.59023998199238,0.));
#7112=CARTESIAN_POINT('',(-18.5778175999297,1.74105979901401,0.));
#7113=CARTESIAN_POINT('Origin',(-18.4845093299966,2.73669706567396,0.));
#7114=CARTESIAN_POINT('',(-18.5778175999297,1.74105979901401,13.));
#7115=CARTESIAN_POINT('',(-18.5778175999297,1.74105979901401,0.));
#7116=CARTESIAN_POINT('',(-17.4952923049513,2.59023998199238,13.));
#7117=CARTESIAN_POINT('Origin',(-18.4845093299966,2.73669706567396,13.));
#7118=CARTESIAN_POINT('',(-17.4952923049513,2.59023998199238,0.));
#7119=CARTESIAN_POINT('Origin',(-17.5988843254813,1.64931697933719,0.));
#7120=CARTESIAN_POINT('',(-18.7118598491961,1.75362185428837,0.));
#7121=CARTESIAN_POINT('',(-17.5988843254813,1.64931697933719,0.));
#7122=CARTESIAN_POINT('',(-18.7118598491961,1.75362185428837,13.));
#7123=CARTESIAN_POINT('',(-18.7118598491961,1.75362185428837,0.));
#7124=CARTESIAN_POINT('',(-8.79944216274063,0.824658489668592,13.));
#7125=CARTESIAN_POINT('Origin',(-18.4254989505611,3.10927393821618,0.));
#7126=CARTESIAN_POINT('',(-17.4394399250575,2.9428780301451,13.));
#7127=CARTESIAN_POINT('',(-18.2065715530743,4.08501508966447,13.));
#7128=CARTESIAN_POINT('Origin',(-18.4254989505611,3.10927393821618,13.));
#7129=CARTESIAN_POINT('',(-18.2065715530743,4.08501508966447,0.));
#7130=CARTESIAN_POINT('',(-18.2065715530743,4.08501508966447,0.));
#7131=CARTESIAN_POINT('',(-17.4394399250575,2.9428780301451,0.));
#7132=CARTESIAN_POINT('Origin',(-18.4254989505611,3.10927393821618,0.));
#7133=CARTESIAN_POINT('',(-17.4394399250575,2.9428780301451,0.));
#7134=CARTESIAN_POINT('Origin',(-18.337935196262,4.11448919812531,0.));
#7135=CARTESIAN_POINT('',(-18.337935196262,4.11448919812531,13.));
#7136=CARTESIAN_POINT('',(-9.16896759813102,2.05724459906266,13.));
#7137=CARTESIAN_POINT('',(-18.337935196262,4.11448919812531,0.));
#7138=CARTESIAN_POINT('',(-18.337935196262,4.11448919812531,0.));
#7139=CARTESIAN_POINT('',(-17.2472005929999,3.86976067797773,0.));
#7140=CARTESIAN_POINT('Origin',(-16.7341271470625,8.31478109308627,0.));
#7141=CARTESIAN_POINT('',(-15.8385835771673,7.86980725742929,0.));
#7142=CARTESIAN_POINT('',(-17.1305374208376,7.39670762388808,0.));
#7143=CARTESIAN_POINT('Origin',(-16.7341271470625,8.31478109308627,0.));
#7144=CARTESIAN_POINT('',(-17.1305374208376,7.39670762388807,13.));
#7145=CARTESIAN_POINT('',(-17.1305374208376,7.39670762388807,0.));
#7146=CARTESIAN_POINT('',(-15.8385835771673,7.86980725742929,13.));
#7147=CARTESIAN_POINT('Origin',(-16.7341271470625,8.31478109308627,13.));
#7148=CARTESIAN_POINT('',(-15.8385835771673,7.86980725742929,0.));
#7149=CARTESIAN_POINT('Origin',(-16.2278666415473,7.00694799924746,0.));
#7150=CARTESIAN_POINT('',(-17.2541372868972,7.45007618140238,0.));
#7151=CARTESIAN_POINT('',(-16.2278666415473,7.00694799924746,0.));
#7152=CARTESIAN_POINT('',(-17.2541372868972,7.45007618140238,13.));
#7153=CARTESIAN_POINT('',(-17.2541372868972,7.45007618140238,0.));
#7154=CARTESIAN_POINT('',(-8.11393332077363,3.50347399962373,13.));
#7155=CARTESIAN_POINT('Origin',(-16.5628723558448,8.65088754544834,0.));
#7156=CARTESIAN_POINT('',(-15.6764936575763,8.18792663645507,13.));
#7157=CARTESIAN_POINT('',(-16.0531394299608,9.51122023939286,13.));
#7158=CARTESIAN_POINT('Origin',(-16.5628723558448,8.65088754544834,13.));
#7159=CARTESIAN_POINT('',(-16.0531394299608,9.51122023939286,0.));
#7160=CARTESIAN_POINT('',(-16.0531394299608,9.51122023939286,0.));
#7161=CARTESIAN_POINT('',(-15.6764936575763,8.18792663645507,0.));
#7162=CARTESIAN_POINT('Origin',(-16.5628723558448,8.65088754544834,0.));
#7163=CARTESIAN_POINT('',(-15.6764936575763,8.18792663645507,0.));
#7164=CARTESIAN_POINT('Origin',(-16.1689656784104,9.57984538049455,0.));
#7165=CARTESIAN_POINT('',(-16.1689656784104,9.57984538049455,13.));
#7166=CARTESIAN_POINT('',(-8.08448283920519,4.78992269024728,13.));
#7167=CARTESIAN_POINT('',(-16.1689656784104,9.57984538049455,0.));
#7168=CARTESIAN_POINT('',(-16.1689656784104,9.57984538049455,0.));
#7169=CARTESIAN_POINT('',(-15.2072406981632,9.01003919792412,0.));
#7170=CARTESIAN_POINT('Origin',(-13.3456920054543,13.0789564146209,0.));
#7171=CARTESIAN_POINT('',(-12.6314839349494,12.3790229663377,0.));
#7172=CARTESIAN_POINT('',(-14.0064008835214,12.3283141706436,0.));
#7173=CARTESIAN_POINT('Origin',(-13.3456920054543,13.0789564146209,0.));
#7174=CARTESIAN_POINT('',(-14.0064008835214,12.3283141706436,13.));
#7175=CARTESIAN_POINT('',(-14.0064008835214,12.3283141706436,0.));
#7176=CARTESIAN_POINT('',(-12.6314839349494,12.3790229663377,13.));
#7177=CARTESIAN_POINT('Origin',(-13.3456920054543,13.0789564146209,13.));
#7178=CARTESIAN_POINT('',(-12.6314839349494,12.3790229663377,0.));
#7179=CARTESIAN_POINT('Origin',(-13.2683523045433,11.678690128714,0.));
#7180=CARTESIAN_POINT('',(-14.1074595503134,12.4172651441477,0.));
#7181=CARTESIAN_POINT('',(-13.2683523045433,11.678690128714,0.));
#7182=CARTESIAN_POINT('',(-14.1074595503134,12.4172651441477,13.));
#7183=CARTESIAN_POINT('',(-14.1074595503134,12.4172651441477,0.));
#7184=CARTESIAN_POINT('',(-6.63417615227163,5.83934506435699,13.));
#7185=CARTESIAN_POINT('Origin',(-13.0789564146209,13.3456920054543,0.));
#7186=CARTESIAN_POINT('',(-12.3790229663377,12.6314839349494,13.));
#7187=CARTESIAN_POINT('',(-12.3283141706436,14.0064008835214,13.));
#7188=CARTESIAN_POINT('Origin',(-13.0789564146209,13.3456920054543,13.));
#7189=CARTESIAN_POINT('',(-12.3283141706436,14.0064008835214,0.));
#7190=CARTESIAN_POINT('',(-12.3283141706436,14.0064008835214,0.));
#7191=CARTESIAN_POINT('',(-12.3790229663377,12.6314839349494,0.));
#7192=CARTESIAN_POINT('Origin',(-13.0789564146209,13.3456920054543,0.));
#7193=CARTESIAN_POINT('',(-12.3790229663377,12.6314839349494,0.));
#7194=CARTESIAN_POINT('Origin',(-12.4172651441477,14.1074595503134,0.));
#7195=CARTESIAN_POINT('',(-12.4172651441477,14.1074595503134,13.));
#7196=CARTESIAN_POINT('',(-6.20863257207387,7.05372977515671,13.));
#7197=CARTESIAN_POINT('',(-12.4172651441477,14.1074595503134,0.));
#7198=CARTESIAN_POINT('',(-12.4172651441477,14.1074595503134,0.));
#7199=CARTESIAN_POINT('',(-11.678690128714,13.2683523045433,0.));
#7200=CARTESIAN_POINT('Origin',(-8.65088754544834,16.5628723558448,0.));
#7201=CARTESIAN_POINT('',(-8.18792663645507,15.6764936575763,0.));
#7202=CARTESIAN_POINT('',(-9.51122023939285,16.0531394299608,0.));
#7203=CARTESIAN_POINT('Origin',(-8.65088754544834,16.5628723558448,0.));
#7204=CARTESIAN_POINT('',(-9.51122023939285,16.0531394299608,13.));
#7205=CARTESIAN_POINT('',(-9.51122023939285,16.0531394299608,0.));
#7206=CARTESIAN_POINT('',(-8.18792663645507,15.6764936575763,13.));
#7207=CARTESIAN_POINT('Origin',(-8.65088754544834,16.5628723558448,13.));
#7208=CARTESIAN_POINT('',(-8.18792663645507,15.6764936575763,0.));
#7209=CARTESIAN_POINT('Origin',(-9.01003919792412,15.2072406981632,0.));
#7210=CARTESIAN_POINT('',(-9.57984538049455,16.1689656784104,0.));
#7211=CARTESIAN_POINT('',(-9.01003919792412,15.2072406981632,0.));
#7212=CARTESIAN_POINT('',(-9.57984538049455,16.1689656784104,13.));
#7213=CARTESIAN_POINT('',(-9.57984538049455,16.1689656784104,0.));
#7214=CARTESIAN_POINT('',(-4.50501959896206,7.6036203490816,13.));
#7215=CARTESIAN_POINT('Origin',(-8.31478109308627,16.7341271470625,0.));
#7216=CARTESIAN_POINT('',(-7.86980725742929,15.8385835771673,13.));
#7217=CARTESIAN_POINT('',(-7.39670762388807,17.1305374208376,13.));
#7218=CARTESIAN_POINT('Origin',(-8.31478109308627,16.7341271470625,13.));
#7219=CARTESIAN_POINT('',(-7.39670762388807,17.1305374208376,0.));
#7220=CARTESIAN_POINT('',(-7.39670762388807,17.1305374208376,0.));
#7221=CARTESIAN_POINT('',(-7.86980725742929,15.8385835771673,0.));
#7222=CARTESIAN_POINT('Origin',(-8.31478109308627,16.7341271470625,0.));
#7223=CARTESIAN_POINT('',(-7.86980725742929,15.8385835771673,0.));
#7224=CARTESIAN_POINT('Origin',(-7.45007618140238,17.2541372868972,0.));
#7225=CARTESIAN_POINT('',(-7.45007618140238,17.2541372868972,13.));
#7226=CARTESIAN_POINT('',(-3.72503809070119,8.62706864344861,13.));
#7227=CARTESIAN_POINT('',(-7.45007618140238,17.2541372868972,0.));
#7228=CARTESIAN_POINT('',(-7.45007618140238,17.2541372868972,0.));
#7229=CARTESIAN_POINT('',(-7.00694799924746,16.2278666415473,0.));
#7230=CARTESIAN_POINT('Origin',(-3.10927393821618,18.4254989505611,0.));
#7231=CARTESIAN_POINT('',(-2.9428780301451,17.4394399250575,0.));
#7232=CARTESIAN_POINT('',(-4.08501508966447,18.2065715530743,0.));
#7233=CARTESIAN_POINT('Origin',(-3.10927393821618,18.4254989505611,0.));
#7234=CARTESIAN_POINT('',(-4.08501508966447,18.2065715530743,13.));
#7235=CARTESIAN_POINT('',(-4.08501508966447,18.2065715530743,0.));
#7236=CARTESIAN_POINT('',(-2.9428780301451,17.4394399250575,13.));
#7237=CARTESIAN_POINT('Origin',(-3.10927393821618,18.4254989505611,13.));
#7238=CARTESIAN_POINT('',(-2.9428780301451,17.4394399250575,0.));
#7239=CARTESIAN_POINT('Origin',(-3.86976067797772,17.2472005929999,0.));
#7240=CARTESIAN_POINT('',(-4.1144891981253,18.337935196262,0.));
#7241=CARTESIAN_POINT('',(-3.86976067797772,17.2472005929999,0.));
#7242=CARTESIAN_POINT('',(-4.1144891981253,18.337935196262,13.));
#7243=CARTESIAN_POINT('',(-4.1144891981253,18.337935196262,0.));
#7244=CARTESIAN_POINT('',(-1.93488033898886,8.62360029649997,13.));
#7245=CARTESIAN_POINT('Origin',(-2.73669706567396,18.4845093299966,0.));
#7246=CARTESIAN_POINT('',(-2.59023998199238,17.4952923049513,13.));
#7247=CARTESIAN_POINT('',(-1.74105979901401,18.5778175999297,13.));
#7248=CARTESIAN_POINT('Origin',(-2.73669706567396,18.4845093299966,13.));
#7249=CARTESIAN_POINT('',(-1.74105979901401,18.5778175999297,0.));
#7250=CARTESIAN_POINT('',(-1.74105979901401,18.5778175999297,0.));
#7251=CARTESIAN_POINT('',(-2.59023998199238,17.4952923049513,0.));
#7252=CARTESIAN_POINT('Origin',(-2.73669706567396,18.4845093299966,0.));
#7253=CARTESIAN_POINT('',(-2.59023998199238,17.4952923049513,0.));
#7254=CARTESIAN_POINT('Origin',(-1.75362185428836,18.7118598491961,0.));
#7255=CARTESIAN_POINT('',(-1.75362185428836,18.7118598491961,13.));
#7256=CARTESIAN_POINT('',(-0.87681092714418,9.35592992459806,13.));
#7257=CARTESIAN_POINT('',(-1.75362185428836,18.7118598491961,0.));
#7258=CARTESIAN_POINT('',(-1.75362185428836,18.7118598491961,0.));
#7259=CARTESIAN_POINT('',(-1.64931697933718,17.5988843254813,0.));
#7260=CARTESIAN_POINT('Origin',(2.73669706567396,18.4845093299966,0.));
#7261=CARTESIAN_POINT('',(2.59023998199238,17.4952923049513,0.));
#7262=CARTESIAN_POINT('',(1.74105979901401,18.5778175999297,0.));
#7263=CARTESIAN_POINT('Origin',(2.73669706567396,18.4845093299966,0.));
#7264=CARTESIAN_POINT('',(1.74105979901401,18.5778175999297,13.));
#7265=CARTESIAN_POINT('',(1.74105979901401,18.5778175999297,0.));
#7266=CARTESIAN_POINT('',(2.59023998199238,17.4952923049513,13.));
#7267=CARTESIAN_POINT('Origin',(2.73669706567396,18.4845093299966,13.));
#7268=CARTESIAN_POINT('',(2.59023998199238,17.4952923049513,0.));
#7269=CARTESIAN_POINT('Origin',(1.64931697933718,17.5988843254813,0.));
#7270=CARTESIAN_POINT('',(1.75362185428837,18.7118598491961,0.));
#7271=CARTESIAN_POINT('',(1.64931697933718,17.5988843254813,0.));
#7272=CARTESIAN_POINT('',(1.75362185428837,18.7118598491961,13.));
#7273=CARTESIAN_POINT('',(1.75362185428837,18.7118598491961,0.));
#7274=CARTESIAN_POINT('',(0.82465848966859,8.79944216274063,13.));
#7275=CARTESIAN_POINT('Origin',(3.10927393821618,18.4254989505611,0.));
#7276=CARTESIAN_POINT('',(2.9428780301451,17.4394399250575,13.));
#7277=CARTESIAN_POINT('',(4.08501508966447,18.2065715530743,13.));
#7278=CARTESIAN_POINT('Origin',(3.10927393821618,18.4254989505611,13.));
#7279=CARTESIAN_POINT('',(4.08501508966447,18.2065715530743,0.));
#7280=CARTESIAN_POINT('',(4.08501508966447,18.2065715530743,0.));
#7281=CARTESIAN_POINT('',(2.9428780301451,17.4394399250575,0.));
#7282=CARTESIAN_POINT('Origin',(3.10927393821618,18.4254989505611,0.));
#7283=CARTESIAN_POINT('',(2.9428780301451,17.4394399250575,0.));
#7284=CARTESIAN_POINT('Origin',(4.11448919812531,18.337935196262,0.));
#7285=CARTESIAN_POINT('',(4.11448919812531,18.337935196262,13.));
#7286=CARTESIAN_POINT('',(2.05724459906266,9.16896759813102,13.));
#7287=CARTESIAN_POINT('',(4.11448919812531,18.337935196262,0.));
#7288=CARTESIAN_POINT('',(4.11448919812531,18.337935196262,0.));
#7289=CARTESIAN_POINT('',(3.86976067797773,17.2472005929999,0.));
#7290=CARTESIAN_POINT('Origin',(8.31478109308627,16.7341271470625,0.));
#7291=CARTESIAN_POINT('',(7.86980725742929,15.8385835771673,0.));
#7292=CARTESIAN_POINT('',(7.39670762388808,17.1305374208376,0.));
#7293=CARTESIAN_POINT('Origin',(8.31478109308627,16.7341271470625,0.));
#7294=CARTESIAN_POINT('',(7.39670762388808,17.1305374208376,13.));
#7295=CARTESIAN_POINT('',(7.39670762388808,17.1305374208376,0.));
#7296=CARTESIAN_POINT('',(7.86980725742929,15.8385835771673,13.));
#7297=CARTESIAN_POINT('Origin',(8.31478109308627,16.7341271470625,13.));
#7298=CARTESIAN_POINT('',(7.86980725742929,15.8385835771673,0.));
#7299=CARTESIAN_POINT('Origin',(7.00694799924747,16.2278666415473,0.));
#7300=CARTESIAN_POINT('',(7.45007618140239,17.2541372868972,0.));
#7301=CARTESIAN_POINT('',(7.00694799924747,16.2278666415473,0.));
#7302=CARTESIAN_POINT('',(7.45007618140239,17.2541372868972,13.));
#7303=CARTESIAN_POINT('',(7.45007618140239,17.2541372868972,0.));
#7304=CARTESIAN_POINT('',(3.50347399962373,8.11393332077363,13.));
#7305=CARTESIAN_POINT('Origin',(8.65088754544834,16.5628723558448,0.));
#7306=CARTESIAN_POINT('',(8.18792663645507,15.6764936575763,13.));
#7307=CARTESIAN_POINT('',(9.51122023939286,16.0531394299608,13.));
#7308=CARTESIAN_POINT('Origin',(8.65088754544834,16.5628723558448,13.));
#7309=CARTESIAN_POINT('',(9.51122023939286,16.0531394299608,0.));
#7310=CARTESIAN_POINT('',(9.51122023939286,16.0531394299608,0.));
#7311=CARTESIAN_POINT('',(8.18792663645507,15.6764936575763,0.));
#7312=CARTESIAN_POINT('Origin',(8.65088754544834,16.5628723558448,0.));
#7313=CARTESIAN_POINT('',(8.18792663645507,15.6764936575763,0.));
#7314=CARTESIAN_POINT('Origin',(9.57984538049455,16.1689656784104,0.));
#7315=CARTESIAN_POINT('',(9.57984538049455,16.1689656784104,13.));
#7316=CARTESIAN_POINT('',(4.78992269024728,8.08448283920519,13.));
#7317=CARTESIAN_POINT('',(9.57984538049455,16.1689656784104,0.));
#7318=CARTESIAN_POINT('',(9.57984538049455,16.1689656784104,0.));
#7319=CARTESIAN_POINT('',(9.01003919792412,15.2072406981632,0.));
#7320=CARTESIAN_POINT('Origin',(13.0789564146209,13.3456920054543,0.));
#7321=CARTESIAN_POINT('',(12.3790229663377,12.6314839349494,0.));
#7322=CARTESIAN_POINT('',(12.3283141706436,14.0064008835214,0.));
#7323=CARTESIAN_POINT('Origin',(13.0789564146209,13.3456920054543,0.));
#7324=CARTESIAN_POINT('',(12.3283141706436,14.0064008835214,13.));
#7325=CARTESIAN_POINT('',(12.3283141706436,14.0064008835214,0.));
#7326=CARTESIAN_POINT('',(12.3790229663377,12.6314839349494,13.));
#7327=CARTESIAN_POINT('Origin',(13.0789564146209,13.3456920054543,13.));
#7328=CARTESIAN_POINT('',(12.3790229663377,12.6314839349494,0.));
#7329=CARTESIAN_POINT('Origin',(11.678690128714,13.2683523045433,0.));
#7330=CARTESIAN_POINT('',(12.4172651441477,14.1074595503134,0.));
#7331=CARTESIAN_POINT('',(11.678690128714,13.2683523045433,0.));
#7332=CARTESIAN_POINT('',(12.4172651441477,14.1074595503134,13.));
#7333=CARTESIAN_POINT('',(12.4172651441477,14.1074595503134,0.));
#7334=CARTESIAN_POINT('',(5.839345064357,6.63417615227163,13.));
#7335=CARTESIAN_POINT('Origin',(13.3456920054543,13.0789564146209,0.));
#7336=CARTESIAN_POINT('',(12.6314839349494,12.3790229663377,13.));
#7337=CARTESIAN_POINT('',(14.0064008835214,12.3283141706436,13.));
#7338=CARTESIAN_POINT('Origin',(13.3456920054543,13.0789564146209,13.));
#7339=CARTESIAN_POINT('',(14.0064008835214,12.3283141706436,0.));
#7340=CARTESIAN_POINT('',(14.0064008835214,12.3283141706436,0.));
#7341=CARTESIAN_POINT('',(12.6314839349494,12.3790229663377,0.));
#7342=CARTESIAN_POINT('Origin',(13.3456920054543,13.0789564146209,0.));
#7343=CARTESIAN_POINT('',(12.6314839349494,12.3790229663377,0.));
#7344=CARTESIAN_POINT('Origin',(14.1074595503134,12.4172651441477,0.));
#7345=CARTESIAN_POINT('',(14.1074595503134,12.4172651441477,13.));
#7346=CARTESIAN_POINT('',(7.05372977515671,6.20863257207387,13.));
#7347=CARTESIAN_POINT('',(14.1074595503134,12.4172651441477,0.));
#7348=CARTESIAN_POINT('',(14.1074595503134,12.4172651441477,0.));
#7349=CARTESIAN_POINT('',(13.2683523045433,11.678690128714,0.));
#7350=CARTESIAN_POINT('Origin',(16.5628723558448,8.65088754544834,0.));
#7351=CARTESIAN_POINT('',(15.6764936575763,8.18792663645507,0.));
#7352=CARTESIAN_POINT('',(16.0531394299608,9.51122023939286,0.));
#7353=CARTESIAN_POINT('Origin',(16.5628723558448,8.65088754544834,0.));
#7354=CARTESIAN_POINT('',(16.0531394299608,9.51122023939286,13.));
#7355=CARTESIAN_POINT('',(16.0531394299608,9.51122023939286,0.));
#7356=CARTESIAN_POINT('',(15.6764936575763,8.18792663645507,13.));
#7357=CARTESIAN_POINT('Origin',(16.5628723558448,8.65088754544834,13.));
#7358=CARTESIAN_POINT('',(15.6764936575763,8.18792663645507,0.));
#7359=CARTESIAN_POINT('Origin',(15.2072406981632,9.01003919792412,0.));
#7360=CARTESIAN_POINT('',(16.1689656784104,9.57984538049455,0.));
#7361=CARTESIAN_POINT('',(15.2072406981632,9.01003919792412,0.));
#7362=CARTESIAN_POINT('',(16.1689656784104,9.57984538049455,13.));
#7363=CARTESIAN_POINT('',(16.1689656784104,9.57984538049455,0.));
#7364=CARTESIAN_POINT('',(7.6036203490816,4.50501959896206,13.));
#7365=CARTESIAN_POINT('Origin',(16.7341271470625,8.31478109308627,0.));
#7366=CARTESIAN_POINT('',(15.8385835771673,7.86980725742929,13.));
#7367=CARTESIAN_POINT('',(17.1305374208376,7.39670762388807,13.));
#7368=CARTESIAN_POINT('Origin',(16.7341271470625,8.31478109308627,13.));
#7369=CARTESIAN_POINT('',(17.1305374208376,7.39670762388807,0.));
#7370=CARTESIAN_POINT('',(17.1305374208376,7.39670762388807,0.));
#7371=CARTESIAN_POINT('',(15.8385835771673,7.86980725742929,0.));
#7372=CARTESIAN_POINT('Origin',(16.7341271470625,8.31478109308627,0.));
#7373=CARTESIAN_POINT('',(15.8385835771673,7.86980725742929,0.));
#7374=CARTESIAN_POINT('Origin',(17.2541372868972,7.45007618140238,0.));
#7375=CARTESIAN_POINT('',(17.2541372868972,7.45007618140238,13.));
#7376=CARTESIAN_POINT('',(8.62706864344861,3.72503809070119,13.));
#7377=CARTESIAN_POINT('',(17.2541372868972,7.45007618140238,0.));
#7378=CARTESIAN_POINT('',(17.2541372868972,7.45007618140238,0.));
#7379=CARTESIAN_POINT('',(16.2278666415473,7.00694799924746,0.));
#7380=CARTESIAN_POINT('Origin',(18.4254989505611,3.10927393821618,0.));
#7381=CARTESIAN_POINT('',(17.4394399250575,2.9428780301451,0.));
#7382=CARTESIAN_POINT('',(18.2065715530743,4.08501508966447,0.));
#7383=CARTESIAN_POINT('Origin',(18.4254989505611,3.10927393821618,0.));
#7384=CARTESIAN_POINT('',(18.2065715530743,4.08501508966447,13.));
#7385=CARTESIAN_POINT('',(18.2065715530743,4.08501508966447,0.));
#7386=CARTESIAN_POINT('',(17.4394399250575,2.9428780301451,13.));
#7387=CARTESIAN_POINT('Origin',(18.4254989505611,3.10927393821618,13.));
#7388=CARTESIAN_POINT('',(17.4394399250575,2.9428780301451,0.));
#7389=CARTESIAN_POINT('Origin',(17.2472005929999,3.86976067797773,0.));
#7390=CARTESIAN_POINT('',(18.337935196262,4.1144891981253,0.));
#7391=CARTESIAN_POINT('',(17.2472005929999,3.86976067797773,0.));
#7392=CARTESIAN_POINT('',(18.337935196262,4.1144891981253,13.));
#7393=CARTESIAN_POINT('',(18.337935196262,4.1144891981253,0.));
#7394=CARTESIAN_POINT('',(8.62360029649997,1.93488033898886,13.));
#7395=CARTESIAN_POINT('Ctrl Pts',(21.1275013067528,-6.13422273260091,0.));
#7396=CARTESIAN_POINT('Ctrl Pts',(21.1275013067528,-6.13422273260091,21.));
#7397=CARTESIAN_POINT('Ctrl Pts',(21.1204271980506,-6.12649903511518,0.));
#7398=CARTESIAN_POINT('Ctrl Pts',(21.1204271980506,-6.12649903511518,21.));
#7399=CARTESIAN_POINT('Ctrl Pts',(21.1062663590356,-6.11107360216958,0.));
#7400=CARTESIAN_POINT('Ctrl Pts',(21.1062663590356,-6.11107360216958,21.));
#7401=CARTESIAN_POINT('Ctrl Pts',(21.0849872356853,-6.08800133883115,0.));
#7402=CARTESIAN_POINT('Ctrl Pts',(21.0849872356853,-6.08800133883115,21.));
#7403=CARTESIAN_POINT('Ctrl Pts',(21.0565393163693,-6.05737013696533,0.));
#7404=CARTESIAN_POINT('Ctrl Pts',(21.0565393163693,-6.05737013696533,21.));
#7405=CARTESIAN_POINT('Ctrl Pts',(21.0208530236003,-6.01930117633045,0.));
#7406=CARTESIAN_POINT('Ctrl Pts',(21.0208530236003,-6.01930117633045,21.));
#7407=CARTESIAN_POINT('Ctrl Pts',(20.9850401822713,-5.98145286361837,0.));
#7408=CARTESIAN_POINT('Ctrl Pts',(20.9850401822713,-5.98145286361837,21.));
#7409=CARTESIAN_POINT('Ctrl Pts',(20.9491006734021,-5.94382608200804,0.));
#7410=CARTESIAN_POINT('Ctrl Pts',(20.9491006734021,-5.94382608200804,21.));
#7411=CARTESIAN_POINT('Ctrl Pts',(20.9130344665641,-5.906422006626,0.));
#7412=CARTESIAN_POINT('Ctrl Pts',(20.9130344665641,-5.906422006626,21.));
#7413=CARTESIAN_POINT('Ctrl Pts',(20.8768416821402,-5.86924212736288,0.));
#7414=CARTESIAN_POINT('Ctrl Pts',(20.8768416821402,-5.86924212736288,21.));
#7415=CARTESIAN_POINT('Ctrl Pts',(20.8405225541277,-5.83228817460178,0.));
#7416=CARTESIAN_POINT('Ctrl Pts',(20.8405225541277,-5.83228817460178,21.));
#7417=CARTESIAN_POINT('Ctrl Pts',(20.8040773827343,-5.79556203439644,0.));
#7418=CARTESIAN_POINT('Ctrl Pts',(20.8040773827343,-5.79556203439644,21.));
#7419=CARTESIAN_POINT('Ctrl Pts',(20.7675064905026,-5.75906566327796,0.));
#7420=CARTESIAN_POINT('Ctrl Pts',(20.7675064905026,-5.75906566327796,21.));
#7421=CARTESIAN_POINT('Ctrl Pts',(20.7308101804425,-5.72280100798241,0.));
#7422=CARTESIAN_POINT('Ctrl Pts',(20.7308101804425,-5.72280100798241,21.));
#7423=CARTESIAN_POINT('Ctrl Pts',(20.6939886877061,-5.68676990500164,0.));
#7424=CARTESIAN_POINT('Ctrl Pts',(20.6939886877061,-5.68676990500164,21.));
#7425=CARTESIAN_POINT('Ctrl Pts',(20.6570421847033,-5.65097411164335,0.));
#7426=CARTESIAN_POINT('Ctrl Pts',(20.6570421847033,-5.65097411164335,21.));
#7427=CARTESIAN_POINT('Ctrl Pts',(20.6199707996366,-5.6154153671515,0.));
#7428=CARTESIAN_POINT('Ctrl Pts',(20.6199707996366,-5.6154153671515,21.));
#7429=CARTESIAN_POINT('Ctrl Pts',(20.5827746317185,-5.58009544402475,0.));
#7430=CARTESIAN_POINT('Ctrl Pts',(20.5827746317185,-5.58009544402475,21.));
#7431=CARTESIAN_POINT('Ctrl Pts',(20.5454537676144,-5.5450161968946,0.));
#7432=CARTESIAN_POINT('Ctrl Pts',(20.5454537676144,-5.5450161968946,21.));
#7433=CARTESIAN_POINT('Ctrl Pts',(20.5080083009242,-5.51017962306782,0.));
#7434=CARTESIAN_POINT('Ctrl Pts',(20.5080083009242,-5.51017962306782,21.));
#7435=CARTESIAN_POINT('Ctrl Pts',(20.4704383353718,-5.47558784449851,0.));
#7436=CARTESIAN_POINT('Ctrl Pts',(20.4704383353718,-5.47558784449851,21.));
#7437=CARTESIAN_POINT('Ctrl Pts',(20.4327439816542,-5.44124306065111,0.));
#7438=CARTESIAN_POINT('Ctrl Pts',(20.4327439816542,-5.44124306065111,21.));
#7439=CARTESIAN_POINT('Ctrl Pts',(20.3949253578015,-5.40714750595875,0.));
#7440=CARTESIAN_POINT('Ctrl Pts',(20.3949253578015,-5.40714750595875,21.));
#7441=CARTESIAN_POINT('Ctrl Pts',(20.3569825877537,-5.37330341114649,0.));
#7442=CARTESIAN_POINT('Ctrl Pts',(20.3569825877537,-5.37330341114649,21.));
#7443=CARTESIAN_POINT('Ctrl Pts',(20.3189158047642,-5.33971294212214,0.));
#7444=CARTESIAN_POINT('Ctrl Pts',(20.3189158047642,-5.33971294212214,21.));
#7445=CARTESIAN_POINT('Ctrl Pts',(20.2807251380077,-5.30637824220998,0.));
#7446=CARTESIAN_POINT('Ctrl Pts',(20.2807251380077,-5.30637824220998,21.));
#7447=CARTESIAN_POINT('Ctrl Pts',(20.2424106921768,-5.27330152298151,0.));
#7448=CARTESIAN_POINT('Ctrl Pts',(20.2424106921768,-5.27330152298151,21.));
#7449=CARTESIAN_POINT('Ctrl Pts',(20.2039725283917,-5.24048514441891,0.));
#7450=CARTESIAN_POINT('Ctrl Pts',(20.2039725283917,-5.24048514441891,21.));
#7451=CARTESIAN_POINT('Ctrl Pts',(20.1654106491899,-5.20793168386164,0.));
#7452=CARTESIAN_POINT('Ctrl Pts',(20.1654106491899,-5.20793168386164,21.));
#7453=CARTESIAN_POINT('Ctrl Pts',(20.1267249732337,-5.17564404279922,0.));
#7454=CARTESIAN_POINT('Ctrl Pts',(20.1267249732337,-5.17564404279922,21.));
#7455=CARTESIAN_POINT('Ctrl Pts',(20.087915358486,-5.14362537555398,0.));
#7456=CARTESIAN_POINT('Ctrl Pts',(20.087915358486,-5.14362537555398,21.));
#7457=CARTESIAN_POINT('Ctrl Pts',(20.0489816528155,-5.11187891582335,0.));
#7458=CARTESIAN_POINT('Ctrl Pts',(20.0489816528155,-5.11187891582335,21.));
#7459=CARTESIAN_POINT('Ctrl Pts',(20.0099237417205,-5.08040781745337,0.));
#7460=CARTESIAN_POINT('Ctrl Pts',(20.0099237417205,-5.08040781745337,21.));
#7461=CARTESIAN_POINT('Ctrl Pts',(19.9707415879783,-5.04921502064063,0.));
#7462=CARTESIAN_POINT('Ctrl Pts',(19.9707415879783,-5.04921502064063,21.));
#7463=CARTESIAN_POINT('Ctrl Pts',(19.931435301086,-5.01830302225558,0.));
#7464=CARTESIAN_POINT('Ctrl Pts',(19.931435301086,-5.01830302225558,21.));
#7465=CARTESIAN_POINT('Ctrl Pts',(19.8920050831202,-4.98767405031333,0.));
#7466=CARTESIAN_POINT('Ctrl Pts',(19.8920050831202,-4.98767405031333,21.));
#7467=CARTESIAN_POINT('Ctrl Pts',(19.8524510953961,-4.95733049830096,0.));
#7468=CARTESIAN_POINT('Ctrl Pts',(19.8524510953961,-4.95733049830096,21.));
#7469=CARTESIAN_POINT('Ctrl Pts',(19.8127733387903,-4.92727531494347,0.));
#7470=CARTESIAN_POINT('Ctrl Pts',(19.8127733387903,-4.92727531494347,21.));
#7471=CARTESIAN_POINT('Ctrl Pts',(19.772971552601,-4.89751233527805,0.));
#7472=CARTESIAN_POINT('Ctrl Pts',(19.772971552601,-4.89751233527805,21.));
#7473=CARTESIAN_POINT('Ctrl Pts',(19.7330450480715,-4.86804682289087,0.));
#7474=CARTESIAN_POINT('Ctrl Pts',(19.7330450480715,-4.86804682289087,21.));
#7475=CARTESIAN_POINT('Ctrl Pts',(19.6929928227072,-4.83888510708974,0.));
#7476=CARTESIAN_POINT('Ctrl Pts',(19.6929928227072,-4.83888510708974,21.));
#7477=CARTESIAN_POINT('Ctrl Pts',(19.6528138625329,-4.81003361418061,0.));
#7478=CARTESIAN_POINT('Ctrl Pts',(19.6528138625329,-4.81003361418061,21.));
#7479=CARTESIAN_POINT('Ctrl Pts',(19.6125074152527,-4.78149799361731,0.));
#7480=CARTESIAN_POINT('Ctrl Pts',(19.6125074152527,-4.78149799361731,21.));
#7481=CARTESIAN_POINT('Ctrl Pts',(19.5720732205813,-4.75328238194611,0.));
#7482=CARTESIAN_POINT('Ctrl Pts',(19.5720732205813,-4.75328238194611,21.));
#7483=CARTESIAN_POINT('Ctrl Pts',(19.531511899192,-4.72538815796616,0.));
#7484=CARTESIAN_POINT('Ctrl Pts',(19.531511899192,-4.72538815796616,21.));
#7485=CARTESIAN_POINT('Ctrl Pts',(19.4908246636763,-4.69781487613785,0.));
#7486=CARTESIAN_POINT('Ctrl Pts',(19.4908246636763,-4.69781487613785,21.));
#7487=CARTESIAN_POINT('Ctrl Pts',(19.4500125912299,-4.67056260851454,0.));
#7488=CARTESIAN_POINT('Ctrl Pts',(19.4500125912299,-4.67056260851454,21.));
#7489=CARTESIAN_POINT('Ctrl Pts',(19.4090759683639,-4.64363405547472,0.));
#7490=CARTESIAN_POINT('Ctrl Pts',(19.4090759683639,-4.64363405547472,21.));
#7491=CARTESIAN_POINT('Ctrl Pts',(19.3680137353983,-4.61703633725712,0.));
#7492=CARTESIAN_POINT('Ctrl Pts',(19.3680137353983,-4.61703633725712,21.));
#7493=CARTESIAN_POINT('Ctrl Pts',(19.3268225655679,-4.59078395765677,0.));
#7494=CARTESIAN_POINT('Ctrl Pts',(19.3268225655679,-4.59078395765677,21.));
#7495=CARTESIAN_POINT('Ctrl Pts',(19.2854975819105,-4.56489651606741,0.));
#7496=CARTESIAN_POINT('Ctrl Pts',(19.2854975819105,-4.56489651606741,21.));
#7497=CARTESIAN_POINT('Ctrl Pts',(19.2440340196551,-4.53939338835152,0.));
#7498=CARTESIAN_POINT('Ctrl Pts',(19.2440340196551,-4.53939338835152,21.));
#7499=CARTESIAN_POINT('Ctrl Pts',(19.2024287376926,-4.51428889122955,0.));
#7500=CARTESIAN_POINT('Ctrl Pts',(19.2024287376926,-4.51428889122955,21.));
#7501=CARTESIAN_POINT('Ctrl Pts',(19.1606814968494,-4.48958819710577,0.));
#7502=CARTESIAN_POINT('Ctrl Pts',(19.1606814968494,-4.48958819710577,21.));
#7503=CARTESIAN_POINT('Ctrl Pts',(19.1187970904932,-4.46528051067022,0.));
#7504=CARTESIAN_POINT('Ctrl Pts',(19.1187970904932,-4.46528051067022,21.));
#7505=CARTESIAN_POINT('Ctrl Pts',(19.0767833717249,-4.44134542994082,0.));
#7506=CARTESIAN_POINT('Ctrl Pts',(19.0767833717249,-4.44134542994082,21.));
#7507=CARTESIAN_POINT('Ctrl Pts',(19.034647328575,-4.41776558033332,0.));
#7508=CARTESIAN_POINT('Ctrl Pts',(19.034647328575,-4.41776558033332,21.));
#7509=CARTESIAN_POINT('Ctrl Pts',(18.9923914823906,-4.39453820875555,0.));
#7510=CARTESIAN_POINT('Ctrl Pts',(18.9923914823906,-4.39453820875555,21.));
#7511=CARTESIAN_POINT('Ctrl Pts',(18.9500107909187,-4.37168516143123,0.));
#7512=CARTESIAN_POINT('Ctrl Pts',(18.9500107909187,-4.37168516143123,21.));
#7513=CARTESIAN_POINT('Ctrl Pts',(18.9074876952706,-4.34926881342022,0.));
#7514=CARTESIAN_POINT('Ctrl Pts',(18.9074876952706,-4.34926881342022,21.));
#7515=CARTESIAN_POINT('Ctrl Pts',(18.8647973781745,-4.32737526247704,0.));
#7516=CARTESIAN_POINT('Ctrl Pts',(18.8647973781745,-4.32737526247704,21.));
#7517=CARTESIAN_POINT('Ctrl Pts',(18.8219166495975,-4.30608591031526,0.));
#7518=CARTESIAN_POINT('Ctrl Pts',(18.8219166495975,-4.30608591031526,21.));
#7519=CARTESIAN_POINT('Ctrl Pts',(18.778832216358,-4.28545098663153,0.));
#7520=CARTESIAN_POINT('Ctrl Pts',(18.778832216358,-4.28545098663153,21.));
#7521=CARTESIAN_POINT('Ctrl Pts',(18.735547949685,-4.26546636161933,0.));
#7522=CARTESIAN_POINT('Ctrl Pts',(18.735547949685,-4.26546636161933,21.));
#7523=CARTESIAN_POINT('Ctrl Pts',(18.6920958920047,-4.24603817988453,0.));
#7524=CARTESIAN_POINT('Ctrl Pts',(18.6920958920047,-4.24603817988453,21.));
#7525=CARTESIAN_POINT('Ctrl Pts',(18.6485210883348,-4.22703266508919,0.));
#7526=CARTESIAN_POINT('Ctrl Pts',(18.6485210883348,-4.22703266508919,21.));
#7527=CARTESIAN_POINT('Ctrl Pts',(18.6048602364653,-4.20834600700665,0.));
#7528=CARTESIAN_POINT('Ctrl Pts',(18.6048602364653,-4.20834600700665,21.));
#7529=CARTESIAN_POINT('Ctrl Pts',(18.5611217636409,-4.18996967278621,0.));
#7530=CARTESIAN_POINT('Ctrl Pts',(18.5611217636409,-4.18996967278621,21.));
#7531=CARTESIAN_POINT('Ctrl Pts',(18.5172668097744,-4.17205262766562,0.));
#7532=CARTESIAN_POINT('Ctrl Pts',(18.5172668097744,-4.17205262766562,21.));
#7533=CARTESIAN_POINT('Ctrl Pts',(18.4731856794913,-4.15497867673974,0.));
#7534=CARTESIAN_POINT('Ctrl Pts',(18.4731856794913,-4.15497867673974,21.));
#7535=CARTESIAN_POINT('Ctrl Pts',(18.4287286547442,-4.13926275457062,0.));
#7536=CARTESIAN_POINT('Ctrl Pts',(18.4287286547442,-4.13926275457062,21.));
#7537=CARTESIAN_POINT('Ctrl Pts',(18.3927403741815,-4.12819301671079,0.));
#7538=CARTESIAN_POINT('Ctrl Pts',(18.3927403741815,-4.12819301671079,21.));
#7539=CARTESIAN_POINT('Ctrl Pts',(18.3654573320481,-4.1209201986886,0.));
#7540=CARTESIAN_POINT('Ctrl Pts',(18.3654573320481,-4.1209201986886,21.));
#7541=CARTESIAN_POINT('Ctrl Pts',(18.3471320125699,-4.11655269114952,0.));
#7542=CARTESIAN_POINT('Ctrl Pts',(18.3471320125699,-4.11655269114952,21.));
#7543=CARTESIAN_POINT('Ctrl Pts',(18.337935196262,-4.11448919812531,0.));
#7544=CARTESIAN_POINT('Ctrl Pts',(18.337935196262,-4.11448919812531,21.));
#7545=CARTESIAN_POINT('',(21.1275013067528,-6.13422273260085,0.));
#7546=CARTESIAN_POINT('Ctrl Pts',(18.337935196262,-4.11448919812531,0.));
#7547=CARTESIAN_POINT('Ctrl Pts',(18.3471320125699,-4.11655269114952,0.));
#7548=CARTESIAN_POINT('Ctrl Pts',(18.3654573320481,-4.1209201986886,0.));
#7549=CARTESIAN_POINT('Ctrl Pts',(18.3927403741815,-4.12819301671079,0.));
#7550=CARTESIAN_POINT('Ctrl Pts',(18.4287286547442,-4.13926275457062,0.));
#7551=CARTESIAN_POINT('Ctrl Pts',(18.4731856794913,-4.15497867673974,0.));
#7552=CARTESIAN_POINT('Ctrl Pts',(18.5172668097744,-4.17205262766562,0.));
#7553=CARTESIAN_POINT('Ctrl Pts',(18.5611217636409,-4.18996967278621,0.));
#7554=CARTESIAN_POINT('Ctrl Pts',(18.6048602364653,-4.20834600700665,0.));
#7555=CARTESIAN_POINT('Ctrl Pts',(18.6485210883348,-4.22703266508919,0.));
#7556=CARTESIAN_POINT('Ctrl Pts',(18.6920958920047,-4.24603817988453,0.));
#7557=CARTESIAN_POINT('Ctrl Pts',(18.735547949685,-4.26546636161933,0.));
#7558=CARTESIAN_POINT('Ctrl Pts',(18.778832216358,-4.28545098663153,0.));
#7559=CARTESIAN_POINT('Ctrl Pts',(18.8219166495975,-4.30608591031526,0.));
#7560=CARTESIAN_POINT('Ctrl Pts',(18.8647973781745,-4.32737526247704,0.));
#7561=CARTESIAN_POINT('Ctrl Pts',(18.9074876952706,-4.34926881342022,0.));
#7562=CARTESIAN_POINT('Ctrl Pts',(18.9500107909187,-4.37168516143123,0.));
#7563=CARTESIAN_POINT('Ctrl Pts',(18.9923914823906,-4.39453820875555,0.));
#7564=CARTESIAN_POINT('Ctrl Pts',(19.034647328575,-4.41776558033332,0.));
#7565=CARTESIAN_POINT('Ctrl Pts',(19.0767833717249,-4.44134542994082,0.));
#7566=CARTESIAN_POINT('Ctrl Pts',(19.1187970904932,-4.46528051067022,0.));
#7567=CARTESIAN_POINT('Ctrl Pts',(19.1606814968494,-4.48958819710577,0.));
#7568=CARTESIAN_POINT('Ctrl Pts',(19.2024287376926,-4.51428889122955,0.));
#7569=CARTESIAN_POINT('Ctrl Pts',(19.2440340196551,-4.53939338835152,0.));
#7570=CARTESIAN_POINT('Ctrl Pts',(19.2854975819105,-4.56489651606741,0.));
#7571=CARTESIAN_POINT('Ctrl Pts',(19.3268225655679,-4.59078395765677,0.));
#7572=CARTESIAN_POINT('Ctrl Pts',(19.3680137353983,-4.61703633725712,0.));
#7573=CARTESIAN_POINT('Ctrl Pts',(19.4090759683639,-4.64363405547472,0.));
#7574=CARTESIAN_POINT('Ctrl Pts',(19.4500125912299,-4.67056260851454,0.));
#7575=CARTESIAN_POINT('Ctrl Pts',(19.4908246636763,-4.69781487613785,0.));
#7576=CARTESIAN_POINT('Ctrl Pts',(19.531511899192,-4.72538815796616,0.));
#7577=CARTESIAN_POINT('Ctrl Pts',(19.5720732205813,-4.75328238194611,0.));
#7578=CARTESIAN_POINT('Ctrl Pts',(19.6125074152527,-4.78149799361731,0.));
#7579=CARTESIAN_POINT('Ctrl Pts',(19.6528138625329,-4.81003361418061,0.));
#7580=CARTESIAN_POINT('Ctrl Pts',(19.6929928227072,-4.83888510708974,0.));
#7581=CARTESIAN_POINT('Ctrl Pts',(19.7330450480715,-4.86804682289087,0.));
#7582=CARTESIAN_POINT('Ctrl Pts',(19.772971552601,-4.89751233527805,0.));
#7583=CARTESIAN_POINT('Ctrl Pts',(19.8127733387903,-4.92727531494347,0.));
#7584=CARTESIAN_POINT('Ctrl Pts',(19.8524510953961,-4.95733049830096,0.));
#7585=CARTESIAN_POINT('Ctrl Pts',(19.8920050831202,-4.98767405031333,0.));
#7586=CARTESIAN_POINT('Ctrl Pts',(19.931435301086,-5.01830302225558,0.));
#7587=CARTESIAN_POINT('Ctrl Pts',(19.9707415879783,-5.04921502064063,0.));
#7588=CARTESIAN_POINT('Ctrl Pts',(20.0099237417205,-5.08040781745337,0.));
#7589=CARTESIAN_POINT('Ctrl Pts',(20.0489816528155,-5.11187891582335,0.));
#7590=CARTESIAN_POINT('Ctrl Pts',(20.087915358486,-5.14362537555398,0.));
#7591=CARTESIAN_POINT('Ctrl Pts',(20.1267249732337,-5.17564404279922,0.));
#7592=CARTESIAN_POINT('Ctrl Pts',(20.1654106491899,-5.20793168386164,0.));
#7593=CARTESIAN_POINT('Ctrl Pts',(20.2039725283917,-5.24048514441891,0.));
#7594=CARTESIAN_POINT('Ctrl Pts',(20.2424106921768,-5.27330152298151,0.));
#7595=CARTESIAN_POINT('Ctrl Pts',(20.2807251380077,-5.30637824220998,0.));
#7596=CARTESIAN_POINT('Ctrl Pts',(20.3189158047642,-5.33971294212214,0.));
#7597=CARTESIAN_POINT('Ctrl Pts',(20.3569825877537,-5.37330341114649,0.));
#7598=CARTESIAN_POINT('Ctrl Pts',(20.3949253578015,-5.40714750595875,0.));
#7599=CARTESIAN_POINT('Ctrl Pts',(20.4327439816542,-5.44124306065111,0.));
#7600=CARTESIAN_POINT('Ctrl Pts',(20.4704383353718,-5.47558784449851,0.));
#7601=CARTESIAN_POINT('Ctrl Pts',(20.5080083009242,-5.51017962306782,0.));
#7602=CARTESIAN_POINT('Ctrl Pts',(20.5454537676144,-5.5450161968946,0.));
#7603=CARTESIAN_POINT('Ctrl Pts',(20.5827746317185,-5.58009544402475,0.));
#7604=CARTESIAN_POINT('Ctrl Pts',(20.6199707996366,-5.6154153671515,0.));
#7605=CARTESIAN_POINT('Ctrl Pts',(20.6570421847033,-5.65097411164335,0.));
#7606=CARTESIAN_POINT('Ctrl Pts',(20.6939886877061,-5.68676990500164,0.));
#7607=CARTESIAN_POINT('Ctrl Pts',(20.7308101804425,-5.72280100798241,0.));
#7608=CARTESIAN_POINT('Ctrl Pts',(20.7675064905026,-5.75906566327796,0.));
#7609=CARTESIAN_POINT('Ctrl Pts',(20.8040773827343,-5.79556203439644,0.));
#7610=CARTESIAN_POINT('Ctrl Pts',(20.8405225541277,-5.83228817460178,0.));
#7611=CARTESIAN_POINT('Ctrl Pts',(20.8768416821402,-5.86924212736288,0.));
#7612=CARTESIAN_POINT('Ctrl Pts',(20.9130344665641,-5.906422006626,0.));
#7613=CARTESIAN_POINT('Ctrl Pts',(20.9491006734021,-5.94382608200804,0.));
#7614=CARTESIAN_POINT('Ctrl Pts',(20.9850401822713,-5.98145286361837,0.));
#7615=CARTESIAN_POINT('Ctrl Pts',(21.0280155918661,-6.02687083887287,0.));
#7616=CARTESIAN_POINT('Ctrl Pts',(21.0636702474951,-6.06499496148845,0.));
#7617=CARTESIAN_POINT('Ctrl Pts',(21.0920928984154,-6.09567013127872,0.));
#7618=CARTESIAN_POINT('Ctrl Pts',(21.1133530893457,-6.11877533761501,0.));
#7619=CARTESIAN_POINT('Ctrl Pts',(21.1275013067528,-6.13422273260091,0.));
#7620=CARTESIAN_POINT('',(21.1275013067528,-6.13422273260085,13.));
#7621=CARTESIAN_POINT('Ctrl Pts',(21.1275013067528,-6.13422273260091,13.));
#7622=CARTESIAN_POINT('Ctrl Pts',(21.0578559224639,-6.05818207473574,13.));
#7623=CARTESIAN_POINT('Ctrl Pts',(20.9874765040291,-5.98341417184727,13.));
#7624=CARTESIAN_POINT('Ctrl Pts',(20.91635991547,-5.90994468705572,13.));
#7625=CARTESIAN_POINT('Ctrl Pts',(20.7985166473367,-5.78820256793373,13.));
#7626=CARTESIAN_POINT('Ctrl Pts',(20.6786545089329,-5.67003811891004,13.));
#7627=CARTESIAN_POINT('Ctrl Pts',(20.5568062999927,-5.55573863837939,13.));
#7628=CARTESIAN_POINT('Ctrl Pts',(20.4631466220902,-5.46788135574845,13.));
#7629=CARTESIAN_POINT('Ctrl Pts',(20.3683108766313,-5.38230707224949,13.));
#7630=CARTESIAN_POINT('Ctrl Pts',(20.272307558011,-5.29917141503086,13.));
#7631=CARTESIAN_POINT('Ctrl Pts',(20.1689623013743,-5.20967788549041,13.));
#7632=CARTESIAN_POINT('Ctrl Pts',(20.0642651120126,-5.12300396000483,13.));
#7633=CARTESIAN_POINT('Ctrl Pts',(19.9582092065757,-5.03941267542058,13.));
#7634=CARTESIAN_POINT('Ctrl Pts',(19.8994937733358,-4.99313426716769,13.));
#7635=CARTESIAN_POINT('Ctrl Pts',(19.8403635603379,-4.9477958395688,13.));
#7636=CARTESIAN_POINT('Ctrl Pts',(19.780817320786,-4.90344584463339,13.));
#7637=CARTESIAN_POINT('Ctrl Pts',(19.72343623378,-4.86070845370395,13.));
#7638=CARTESIAN_POINT('Ctrl Pts',(19.665666793385,-4.81889538674849,13.));
#7639=CARTESIAN_POINT('Ctrl Pts',(19.607498635726,-4.7780829655059,13.));
#7640=CARTESIAN_POINT('Ctrl Pts',(19.5572235050457,-4.74280851477666,13.));
#7641=CARTESIAN_POINT('Ctrl Pts',(19.5066514991033,-4.70827845306304,13.));
#7642=CARTESIAN_POINT('Ctrl Pts',(19.4557905173051,-4.67449772148844,13.));
#7643=CARTESIAN_POINT('Ctrl Pts',(19.4192898920658,-4.65025481897416,13.));
#7644=CARTESIAN_POINT('Ctrl Pts',(19.382641288743,-4.62639514838843,13.));
#7645=CARTESIAN_POINT('Ctrl Pts',(19.3458364383459,-4.60295743063937,13.));
#7646=CARTESIAN_POINT('Ctrl Pts',(19.309630908347,-4.57990136645455,13.));
#7647=CARTESIAN_POINT('Ctrl Pts',(19.273272273525,-4.55725971984417,13.));
#7648=CARTESIAN_POINT('Ctrl Pts',(19.2367485575731,-4.5350835755811,13.));
#7649=CARTESIAN_POINT('Ctrl Pts',(19.2050803503215,-4.51585555580649,13.));
#7650=CARTESIAN_POINT('Ctrl Pts',(19.1732873013029,-4.49697986255775,13.));
#7651=CARTESIAN_POINT('Ctrl Pts',(19.1413765621579,-4.47844262265296,13.));
#7652=CARTESIAN_POINT('Ctrl Pts',(19.1124727544724,-4.46165213670422,13.));
#7653=CARTESIAN_POINT('Ctrl Pts',(19.0834740456903,-4.4451340112905,13.));
#7654=CARTESIAN_POINT('Ctrl Pts',(19.0543895552964,-4.42886646472448,13.));
#7655=CARTESIAN_POINT('Ctrl Pts',(19.0298903167199,-4.41516354268672,13.));
#7656=CARTESIAN_POINT('Ctrl Pts',(19.0053307306813,-4.40163676089501,13.));
#7657=CARTESIAN_POINT('Ctrl Pts',(18.9807063064772,-4.38830551710826,13.));
#7658=CARTESIAN_POINT('Ctrl Pts',(18.9450720847457,-4.36901375649227,13.));
#7659=CARTESIAN_POINT('Ctrl Pts',(18.9093017976319,-4.35013223002823,13.));
#7660=CARTESIAN_POINT('Ctrl Pts',(18.8733353264261,-4.33187128669082,13.));
#7661=CARTESIAN_POINT('Ctrl Pts',(18.8516029896876,-4.32083731653844,13.));
#7662=CARTESIAN_POINT('Ctrl Pts',(18.829798004179,-4.31003325584325,13.));
#7663=CARTESIAN_POINT('Ctrl Pts',(18.807913802916,-4.29948469303248,13.));
#7664=CARTESIAN_POINT('Ctrl Pts',(18.787730412872,-4.28975595059153,13.));
#7665=CARTESIAN_POINT('Ctrl Pts',(18.7674792481688,-4.28024580001115,13.));
#7666=CARTESIAN_POINT('Ctrl Pts',(18.7471689057697,-4.27093067976999,13.));
#7667=CARTESIAN_POINT('Ctrl Pts',(18.7192299720025,-4.25811678809167,13.));
#7668=CARTESIAN_POINT('Ctrl Pts',(18.6911811213678,-4.24566493398932,13.));
#7669=CARTESIAN_POINT('Ctrl Pts',(18.6630711735883,-4.23343245343576,13.));
#7670=CARTESIAN_POINT('Ctrl Pts',(18.6452377209709,-4.22567194943,13.));
#7671=CARTESIAN_POINT('Ctrl Pts',(18.6273802008519,-4.21799814921869,13.));
#7672=CARTESIAN_POINT('Ctrl Pts',(18.6095026819575,-4.21040342108815,13.));
#7673=CARTESIAN_POINT('Ctrl Pts',(18.5934584408824,-4.2035875060976,13.));
#7674=CARTESIAN_POINT('Ctrl Pts',(18.5773983085029,-4.1968345819819,13.));
#7675=CARTESIAN_POINT('Ctrl Pts',(18.5613135378487,-4.19017810368168,13.));
#7676=CARTESIAN_POINT('Ctrl Pts',(18.5444052404372,-4.18318081927935,13.));
#7677=CARTESIAN_POINT('Ctrl Pts',(18.5274697699669,-4.17628995976621,13.));
#7678=CARTESIAN_POINT('Ctrl Pts',(18.5104789585687,-4.16960404102653,13.));
#7679=CARTESIAN_POINT('Ctrl Pts',(18.4822572583451,-4.15849874475977,13.));
#7680=CARTESIAN_POINT('Ctrl Pts',(18.4538805850219,-4.14796697295268,13.));
#7681=CARTESIAN_POINT('Ctrl Pts',(18.4251735640106,-4.13860964460765,13.));
#7682=CARTESIAN_POINT('Ctrl Pts',(18.4093434909821,-4.13344968074392,13.));
#7683=CARTESIAN_POINT('Ctrl Pts',(18.3934125378936,-4.12864814562055,13.));
#7684=CARTESIAN_POINT('Ctrl Pts',(18.3773590065616,-4.1242788981144,13.));
#7685=CARTESIAN_POINT('Ctrl Pts',(18.3643002867737,-4.1207247406093,13.));
#7686=CARTESIAN_POINT('Ctrl Pts',(18.3511604736845,-4.11745655843684,13.));
#7687=CARTESIAN_POINT('Ctrl Pts',(18.337935196262,-4.11448919812531,13.));
#7688=CARTESIAN_POINT('',(21.1275013067528,-6.13422273260085,0.));
#7689=CARTESIAN_POINT('Origin',(5.38923623413286E-12,-1.75106900012182E-12,
0.));
#7690=CARTESIAN_POINT('',(20.698113262342,-7.45574324794401,0.));
#7691=CARTESIAN_POINT('Origin',(5.38923623413286E-12,-1.75106900012182E-12,
0.));
#7692=CARTESIAN_POINT('',(20.698113262342,-7.45574324794401,13.));
#7693=CARTESIAN_POINT('Origin',(5.38923623413286E-12,-1.75106900012182E-12,
13.));
#7694=CARTESIAN_POINT('',(20.698113262342,-7.45574324794401,0.));
#7695=CARTESIAN_POINT('Ctrl Pts',(17.2541372868972,-7.45007618140239,0.));
#7696=CARTESIAN_POINT('Ctrl Pts',(17.2541372868972,-7.45007618140239,21.));
#7697=CARTESIAN_POINT('Ctrl Pts',(17.2627905583523,-7.45381253347183,0.));
#7698=CARTESIAN_POINT('Ctrl Pts',(17.2627905583523,-7.45381253347183,21.));
#7699=CARTESIAN_POINT('Ctrl Pts',(17.2801832097582,-7.46105049818251,0.));
#7700=CARTESIAN_POINT('Ctrl Pts',(17.2801832097582,-7.46105049818251,21.));
#7701=CARTESIAN_POINT('Ctrl Pts',(17.3065305096784,-7.4712032346092,0.));
#7702=CARTESIAN_POINT('Ctrl Pts',(17.3065305096784,-7.4712032346092,21.));
#7703=CARTESIAN_POINT('Ctrl Pts',(17.3421522689127,-7.48340100912745,0.));
#7704=CARTESIAN_POINT('Ctrl Pts',(17.3421522689127,-7.48340100912745,21.));
#7705=CARTESIAN_POINT('Ctrl Pts',(17.3873563447297,-7.49681774451751,0.));
#7706=CARTESIAN_POINT('Ctrl Pts',(17.3873563447297,-7.49681774451751,21.));
#7707=CARTESIAN_POINT('Ctrl Pts',(17.4330545448126,-7.50891486634214,0.));
#7708=CARTESIAN_POINT('Ctrl Pts',(17.4330545448126,-7.50891486634214,21.));
#7709=CARTESIAN_POINT('Ctrl Pts',(17.4790653226646,-7.52019696747329,0.));
#7710=CARTESIAN_POINT('Ctrl Pts',(17.4790653226646,-7.52019696747329,21.));
#7711=CARTESIAN_POINT('Ctrl Pts',(17.5252518287336,-7.53103903007864,0.));
#7712=CARTESIAN_POINT('Ctrl Pts',(17.5252518287336,-7.53103903007864,21.));
#7713=CARTESIAN_POINT('Ctrl Pts',(17.5715579419204,-7.54158441095318,0.));
#7714=CARTESIAN_POINT('Ctrl Pts',(17.5715579419204,-7.54158441095318,21.));
#7715=CARTESIAN_POINT('Ctrl Pts',(17.6179818599248,-7.55182125346564,0.));
#7716=CARTESIAN_POINT('Ctrl Pts',(17.6179818599248,-7.55182125346564,21.));
#7717=CARTESIAN_POINT('Ctrl Pts',(17.6645549117314,-7.56164400295863,0.));
#7718=CARTESIAN_POINT('Ctrl Pts',(17.6645549117314,-7.56164400295863,21.));
#7719=CARTESIAN_POINT('Ctrl Pts',(17.7113192869136,-7.57091795530424,0.));
#7720=CARTESIAN_POINT('Ctrl Pts',(17.7113192869136,-7.57091795530424,21.));
#7721=CARTESIAN_POINT('Ctrl Pts',(17.7583042294209,-7.57954834582804,0.));
#7722=CARTESIAN_POINT('Ctrl Pts',(17.7583042294209,-7.57954834582804,21.));
#7723=CARTESIAN_POINT('Ctrl Pts',(17.8055090348024,-7.58752955799499,0.));
#7724=CARTESIAN_POINT('Ctrl Pts',(17.8055090348024,-7.58752955799499,21.));
#7725=CARTESIAN_POINT('Ctrl Pts',(17.8529149331931,-7.59491004201956,0.));
#7726=CARTESIAN_POINT('Ctrl Pts',(17.8529149331931,-7.59491004201956,21.));
#7727=CARTESIAN_POINT('Ctrl Pts',(17.900492838997,-7.60176928403059,0.));
#7728=CARTESIAN_POINT('Ctrl Pts',(17.900492838997,-7.60176928403059,21.));
#7729=CARTESIAN_POINT('Ctrl Pts',(17.9482122228183,-7.60819152580111,0.));
#7730=CARTESIAN_POINT('Ctrl Pts',(17.9482122228183,-7.60819152580111,21.));
#7731=CARTESIAN_POINT('Ctrl Pts',(17.9960506269561,-7.61423755067038,0.));
#7732=CARTESIAN_POINT('Ctrl Pts',(17.9960506269561,-7.61423755067038,21.));
#7733=CARTESIAN_POINT('Ctrl Pts',(18.0439992897906,-7.61992799636654,0.));
#7734=CARTESIAN_POINT('Ctrl Pts',(18.0439992897906,-7.61992799636654,21.));
#7735=CARTESIAN_POINT('Ctrl Pts',(18.0920577897363,-7.62525915358074,0.));
#7736=CARTESIAN_POINT('Ctrl Pts',(18.0920577897363,-7.62525915358074,21.));
#7737=CARTESIAN_POINT('Ctrl Pts',(18.1402306858819,-7.63021285851762,0.));
#7738=CARTESIAN_POINT('Ctrl Pts',(18.1402306858819,-7.63021285851762,21.));
#7739=CARTESIAN_POINT('Ctrl Pts',(18.1885236169197,-7.63476798969017,0.));
#7740=CARTESIAN_POINT('Ctrl Pts',(18.1885236169197,-7.63476798969017,21.));
#7741=CARTESIAN_POINT('Ctrl Pts',(18.2369390502576,-7.63891299603827,0.));
#7742=CARTESIAN_POINT('Ctrl Pts',(18.2369390502576,-7.63891299603827,21.));
#7743=CARTESIAN_POINT('Ctrl Pts',(18.2854741391282,-7.6426522027076,0.));
#7744=CARTESIAN_POINT('Ctrl Pts',(18.2854741391282,-7.6426522027076,21.));
#7745=CARTESIAN_POINT('Ctrl Pts',(18.3341230095852,-7.64599903846601,0.));
#7746=CARTESIAN_POINT('Ctrl Pts',(18.3341230095852,-7.64599903846601,21.));
#7747=CARTESIAN_POINT('Ctrl Pts',(18.3828781275628,-7.6489719793775,0.));
#7748=CARTESIAN_POINT('Ctrl Pts',(18.3828781275628,-7.6489719793775,21.));
#7749=CARTESIAN_POINT('Ctrl Pts',(18.4317319183719,-7.65158974829127,0.));
#7750=CARTESIAN_POINT('Ctrl Pts',(18.4317319183719,-7.65158974829127,21.));
#7751=CARTESIAN_POINT('Ctrl Pts',(18.4806785483052,-7.65386603444743,0.));
#7752=CARTESIAN_POINT('Ctrl Pts',(18.4806785483052,-7.65386603444743,21.));
#7753=CARTESIAN_POINT('Ctrl Pts',(18.5297146894905,-7.65580722110437,0.));
#7754=CARTESIAN_POINT('Ctrl Pts',(18.5297146894905,-7.65580722110437,21.));
#7755=CARTESIAN_POINT('Ctrl Pts',(18.5788385228928,-7.65741532450727,0.));
#7756=CARTESIAN_POINT('Ctrl Pts',(18.5788385228928,-7.65741532450727,21.));
#7757=CARTESIAN_POINT('Ctrl Pts',(18.6280491346907,-7.65868976978872,0.));
#7758=CARTESIAN_POINT('Ctrl Pts',(18.6280491346907,-7.65868976978872,21.));
#7759=CARTESIAN_POINT('Ctrl Pts',(18.6773458057584,-7.65962948375622,0.));
#7760=CARTESIAN_POINT('Ctrl Pts',(18.6773458057584,-7.65962948375622,21.));
#7761=CARTESIAN_POINT('Ctrl Pts',(18.7267272235231,-7.66023521705905,0.));
#7762=CARTESIAN_POINT('Ctrl Pts',(18.7267272235231,-7.66023521705905,21.));
#7763=CARTESIAN_POINT('Ctrl Pts',(18.7761911671591,-7.66051046922541,0.));
#7764=CARTESIAN_POINT('Ctrl Pts',(18.7761911671591,-7.66051046922541,21.));
#7765=CARTESIAN_POINT('Ctrl Pts',(18.8257349246207,-7.66046025294775,0.));
#7766=CARTESIAN_POINT('Ctrl Pts',(18.8257349246207,-7.66046025294775,21.));
#7767=CARTESIAN_POINT('Ctrl Pts',(18.8753555389435,-7.66009036321663,0.));
#7768=CARTESIAN_POINT('Ctrl Pts',(18.8753555389435,-7.66009036321663,21.));
#7769=CARTESIAN_POINT('Ctrl Pts',(18.9250501008887,-7.65940650980099,0.));
#7770=CARTESIAN_POINT('Ctrl Pts',(18.9250501008887,-7.65940650980099,21.));
#7771=CARTESIAN_POINT('Ctrl Pts',(18.974816073814,-7.65841335587266,0.));
#7772=CARTESIAN_POINT('Ctrl Pts',(18.974816073814,-7.65841335587266,21.));
#7773=CARTESIAN_POINT('Ctrl Pts',(19.0246514144531,-7.65711415727855,0.));
#7774=CARTESIAN_POINT('Ctrl Pts',(19.0246514144531,-7.65711415727855,21.));
#7775=CARTESIAN_POINT('Ctrl Pts',(19.0745543888799,-7.65551129907202,0.));
#7776=CARTESIAN_POINT('Ctrl Pts',(19.0745543888799,-7.65551129907202,21.));
#7777=CARTESIAN_POINT('Ctrl Pts',(19.1245234597312,-7.65360662280609,0.));
#7778=CARTESIAN_POINT('Ctrl Pts',(19.1245234597312,-7.65360662280609,21.));
#7779=CARTESIAN_POINT('Ctrl Pts',(19.1745571539291,-7.65140181220526,0.));
#7780=CARTESIAN_POINT('Ctrl Pts',(19.1745571539291,-7.65140181220526,21.));
#7781=CARTESIAN_POINT('Ctrl Pts',(19.224653915265,-7.64889882291924,0.));
#7782=CARTESIAN_POINT('Ctrl Pts',(19.224653915265,-7.64889882291924,21.));
#7783=CARTESIAN_POINT('Ctrl Pts',(19.2748120456486,-7.64610005549614,0.));
#7784=CARTESIAN_POINT('Ctrl Pts',(19.2748120456486,-7.64610005549614,21.));
#7785=CARTESIAN_POINT('Ctrl Pts',(19.3250297839295,-7.64300812875339,0.));
#7786=CARTESIAN_POINT('Ctrl Pts',(19.3250297839295,-7.64300812875339,21.));
#7787=CARTESIAN_POINT('Ctrl Pts',(19.3753053524647,-7.63962574822761,0.));
#7788=CARTESIAN_POINT('Ctrl Pts',(19.3753053524647,-7.63962574822761,21.));
#7789=CARTESIAN_POINT('Ctrl Pts',(19.4256370121006,-7.63595554930654,0.));
#7790=CARTESIAN_POINT('Ctrl Pts',(19.4256370121006,-7.63595554930654,21.));
#7791=CARTESIAN_POINT('Ctrl Pts',(19.4760231231881,-7.63199992715366,0.));
#7792=CARTESIAN_POINT('Ctrl Pts',(19.4760231231881,-7.63199992715366,21.));
#7793=CARTESIAN_POINT('Ctrl Pts',(19.5264621687521,-7.62776096538883,0.));
#7794=CARTESIAN_POINT('Ctrl Pts',(19.5264621687521,-7.62776096538883,21.));
#7795=CARTESIAN_POINT('Ctrl Pts',(19.5769527121826,-7.6232405373522,0.));
#7796=CARTESIAN_POINT('Ctrl Pts',(19.5769527121826,-7.6232405373522,21.));
#7797=CARTESIAN_POINT('Ctrl Pts',(19.6274933688524,-7.61844037070591,0.));
#7798=CARTESIAN_POINT('Ctrl Pts',(19.6274933688524,-7.61844037070591,21.));
#7799=CARTESIAN_POINT('Ctrl Pts',(19.6780827744426,-7.61336212350879,0.));
#7800=CARTESIAN_POINT('Ctrl Pts',(19.6780827744426,-7.61336212350879,21.));
#7801=CARTESIAN_POINT('Ctrl Pts',(19.7287195480601,-7.60800746969262,0.));
#7802=CARTESIAN_POINT('Ctrl Pts',(19.7287195480601,-7.60800746969262,21.));
#7803=CARTESIAN_POINT('Ctrl Pts',(19.7794022782484,-7.60237814110187,0.));
#7804=CARTESIAN_POINT('Ctrl Pts',(19.7794022782484,-7.60237814110187,21.));
#7805=CARTESIAN_POINT('Ctrl Pts',(19.830129556152,-7.59647587605448,0.));
#7806=CARTESIAN_POINT('Ctrl Pts',(19.830129556152,-7.59647587605448,21.));
#7807=CARTESIAN_POINT('Ctrl Pts',(19.8808999994024,-7.59030238888852,0.));
#7808=CARTESIAN_POINT('Ctrl Pts',(19.8808999994024,-7.59030238888852,21.));
#7809=CARTESIAN_POINT('Ctrl Pts',(19.931712276832,-7.58385933533352,0.));
#7810=CARTESIAN_POINT('Ctrl Pts',(19.931712276832,-7.58385933533352,21.));
#7811=CARTESIAN_POINT('Ctrl Pts',(19.9825651387294,-7.57714827622806,0.));
#7812=CARTESIAN_POINT('Ctrl Pts',(19.9825651387294,-7.57714827622806,21.));
#7813=CARTESIAN_POINT('Ctrl Pts',(20.0334574248556,-7.57017066105973,0.));
#7814=CARTESIAN_POINT('Ctrl Pts',(20.0334574248556,-7.57017066105973,21.));
#7815=CARTESIAN_POINT('Ctrl Pts',(20.0843880130978,-7.56292786549461,0.));
#7816=CARTESIAN_POINT('Ctrl Pts',(20.0843880130978,-7.56292786549461,21.));
#7817=CARTESIAN_POINT('Ctrl Pts',(20.1353557774357,-7.55542122125495,0.));
#7818=CARTESIAN_POINT('Ctrl Pts',(20.1353557774357,-7.55542122125495,21.));
#7819=CARTESIAN_POINT('Ctrl Pts',(20.1863595454674,-7.54765204869255,0.));
#7820=CARTESIAN_POINT('Ctrl Pts',(20.1863595454674,-7.54765204869255,21.));
#7821=CARTESIAN_POINT('Ctrl Pts',(20.2373980474879,-7.53962169534167,0.));
#7822=CARTESIAN_POINT('Ctrl Pts',(20.2373980474879,-7.53962169534167,21.));
#7823=CARTESIAN_POINT('Ctrl Pts',(20.2884698940944,-7.53133155804008,0.));
#7824=CARTESIAN_POINT('Ctrl Pts',(20.2884698940944,-7.53133155804008,21.));
#7825=CARTESIAN_POINT('Ctrl Pts',(20.3395736743243,-7.52278303006887,0.));
#7826=CARTESIAN_POINT('Ctrl Pts',(20.3395736743243,-7.52278303006887,21.));
#7827=CARTESIAN_POINT('Ctrl Pts',(20.3907080367098,-7.51397746081994,0.));
#7828=CARTESIAN_POINT('Ctrl Pts',(20.3907080367098,-7.51397746081994,21.));
#7829=CARTESIAN_POINT('Ctrl Pts',(20.4418717748497,-7.50491611266253,0.));
#7830=CARTESIAN_POINT('Ctrl Pts',(20.4418717748497,-7.50491611266253,21.));
#7831=CARTESIAN_POINT('Ctrl Pts',(20.493063915616,-7.49560012018406,0.));
#7832=CARTESIAN_POINT('Ctrl Pts',(20.493063915616,-7.49560012018406,21.));
#7833=CARTESIAN_POINT('Ctrl Pts',(20.5442837929044,-7.48603045196745,0.));
#7834=CARTESIAN_POINT('Ctrl Pts',(20.5442837929044,-7.48603045196745,21.));
#7835=CARTESIAN_POINT('Ctrl Pts',(20.5955309838521,-7.47620789245428,0.));
#7836=CARTESIAN_POINT('Ctrl Pts',(20.5955309838521,-7.47620789245428,21.));
#7837=CARTESIAN_POINT('Ctrl Pts',(20.6365504027501,-7.46814799701906,0.));
#7838=CARTESIAN_POINT('Ctrl Pts',(20.6365504027501,-7.46814799701906,21.));
#7839=CARTESIAN_POINT('Ctrl Pts',(20.6673271112931,-7.46198969876654,0.));
#7840=CARTESIAN_POINT('Ctrl Pts',(20.6673271112931,-7.46198969876654,21.));
#7841=CARTESIAN_POINT('Ctrl Pts',(20.6878503127065,-7.45783379370108,0.));
#7842=CARTESIAN_POINT('Ctrl Pts',(20.6878503127065,-7.45783379370108,21.));
#7843=CARTESIAN_POINT('Ctrl Pts',(20.698113262342,-7.45574324794401,0.));
#7844=CARTESIAN_POINT('Ctrl Pts',(20.698113262342,-7.45574324794401,21.));
#7845=CARTESIAN_POINT('Ctrl Pts',(17.2541372868972,-7.45007618140239,0.));
#7846=CARTESIAN_POINT('Ctrl Pts',(17.2627905583523,-7.45381253347183,0.));
#7847=CARTESIAN_POINT('Ctrl Pts',(17.2801832097582,-7.46105049818251,0.));
#7848=CARTESIAN_POINT('Ctrl Pts',(17.3065305096784,-7.4712032346092,0.));
#7849=CARTESIAN_POINT('Ctrl Pts',(17.3421522689127,-7.48340100912745,0.));
#7850=CARTESIAN_POINT('Ctrl Pts',(17.3873563447297,-7.49681774451751,0.));
#7851=CARTESIAN_POINT('Ctrl Pts',(17.4330545448126,-7.50891486634214,0.));
#7852=CARTESIAN_POINT('Ctrl Pts',(17.4790653226646,-7.52019696747329,0.));
#7853=CARTESIAN_POINT('Ctrl Pts',(17.5252518287336,-7.53103903007864,0.));
#7854=CARTESIAN_POINT('Ctrl Pts',(17.5715579419204,-7.54158441095318,0.));
#7855=CARTESIAN_POINT('Ctrl Pts',(17.6179818599248,-7.55182125346564,0.));
#7856=CARTESIAN_POINT('Ctrl Pts',(17.6645549117314,-7.56164400295863,0.));
#7857=CARTESIAN_POINT('Ctrl Pts',(17.7113192869136,-7.57091795530424,0.));
#7858=CARTESIAN_POINT('Ctrl Pts',(17.7583042294209,-7.57954834582804,0.));
#7859=CARTESIAN_POINT('Ctrl Pts',(17.8055090348024,-7.58752955799499,0.));
#7860=CARTESIAN_POINT('Ctrl Pts',(17.8529149331931,-7.59491004201956,0.));
#7861=CARTESIAN_POINT('Ctrl Pts',(17.900492838997,-7.60176928403059,0.));
#7862=CARTESIAN_POINT('Ctrl Pts',(17.9482122228183,-7.60819152580111,0.));
#7863=CARTESIAN_POINT('Ctrl Pts',(17.9960506269561,-7.61423755067038,0.));
#7864=CARTESIAN_POINT('Ctrl Pts',(18.0439992897906,-7.61992799636654,0.));
#7865=CARTESIAN_POINT('Ctrl Pts',(18.0920577897363,-7.62525915358074,0.));
#7866=CARTESIAN_POINT('Ctrl Pts',(18.1402306858819,-7.63021285851762,0.));
#7867=CARTESIAN_POINT('Ctrl Pts',(18.1885236169197,-7.63476798969017,0.));
#7868=CARTESIAN_POINT('Ctrl Pts',(18.2369390502576,-7.63891299603827,0.));
#7869=CARTESIAN_POINT('Ctrl Pts',(18.2854741391282,-7.6426522027076,0.));
#7870=CARTESIAN_POINT('Ctrl Pts',(18.3341230095852,-7.64599903846601,0.));
#7871=CARTESIAN_POINT('Ctrl Pts',(18.3828781275628,-7.6489719793775,0.));
#7872=CARTESIAN_POINT('Ctrl Pts',(18.4317319183719,-7.65158974829127,0.));
#7873=CARTESIAN_POINT('Ctrl Pts',(18.4806785483052,-7.65386603444743,0.));
#7874=CARTESIAN_POINT('Ctrl Pts',(18.5297146894905,-7.65580722110437,0.));
#7875=CARTESIAN_POINT('Ctrl Pts',(18.5788385228928,-7.65741532450727,0.));
#7876=CARTESIAN_POINT('Ctrl Pts',(18.6280491346907,-7.65868976978872,0.));
#7877=CARTESIAN_POINT('Ctrl Pts',(18.6773458057584,-7.65962948375622,0.));
#7878=CARTESIAN_POINT('Ctrl Pts',(18.7267272235231,-7.66023521705905,0.));
#7879=CARTESIAN_POINT('Ctrl Pts',(18.7761911671591,-7.66051046922541,0.));
#7880=CARTESIAN_POINT('Ctrl Pts',(18.8257349246207,-7.66046025294775,0.));
#7881=CARTESIAN_POINT('Ctrl Pts',(18.8753555389435,-7.66009036321663,0.));
#7882=CARTESIAN_POINT('Ctrl Pts',(18.9250501008887,-7.65940650980099,0.));
#7883=CARTESIAN_POINT('Ctrl Pts',(18.974816073814,-7.65841335587266,0.));
#7884=CARTESIAN_POINT('Ctrl Pts',(19.0246514144531,-7.65711415727855,0.));
#7885=CARTESIAN_POINT('Ctrl Pts',(19.0745543888799,-7.65551129907202,0.));
#7886=CARTESIAN_POINT('Ctrl Pts',(19.1245234597312,-7.65360662280609,0.));
#7887=CARTESIAN_POINT('Ctrl Pts',(19.1745571539291,-7.65140181220526,0.));
#7888=CARTESIAN_POINT('Ctrl Pts',(19.224653915265,-7.64889882291924,0.));
#7889=CARTESIAN_POINT('Ctrl Pts',(19.2748120456486,-7.64610005549614,0.));
#7890=CARTESIAN_POINT('Ctrl Pts',(19.3250297839295,-7.64300812875339,0.));
#7891=CARTESIAN_POINT('Ctrl Pts',(19.3753053524647,-7.63962574822761,0.));
#7892=CARTESIAN_POINT('Ctrl Pts',(19.4256370121006,-7.63595554930654,0.));
#7893=CARTESIAN_POINT('Ctrl Pts',(19.4760231231881,-7.63199992715366,0.));
#7894=CARTESIAN_POINT('Ctrl Pts',(19.5264621687521,-7.62776096538883,0.));
#7895=CARTESIAN_POINT('Ctrl Pts',(19.5769527121826,-7.6232405373522,0.));
#7896=CARTESIAN_POINT('Ctrl Pts',(19.6274933688524,-7.61844037070591,0.));
#7897=CARTESIAN_POINT('Ctrl Pts',(19.6780827744426,-7.61336212350879,0.));
#7898=CARTESIAN_POINT('Ctrl Pts',(19.7287195480601,-7.60800746969262,0.));
#7899=CARTESIAN_POINT('Ctrl Pts',(19.7794022782484,-7.60237814110187,0.));
#7900=CARTESIAN_POINT('Ctrl Pts',(19.830129556152,-7.59647587605448,0.));
#7901=CARTESIAN_POINT('Ctrl Pts',(19.8808999994024,-7.59030238888852,0.));
#7902=CARTESIAN_POINT('Ctrl Pts',(19.931712276832,-7.58385933533352,0.));
#7903=CARTESIAN_POINT('Ctrl Pts',(19.9825651387294,-7.57714827622806,0.));
#7904=CARTESIAN_POINT('Ctrl Pts',(20.0334574248556,-7.57017066105973,0.));
#7905=CARTESIAN_POINT('Ctrl Pts',(20.0843880130978,-7.56292786549461,0.));
#7906=CARTESIAN_POINT('Ctrl Pts',(20.1353557774357,-7.55542122125495,0.));
#7907=CARTESIAN_POINT('Ctrl Pts',(20.1863595454674,-7.54765204869255,0.));
#7908=CARTESIAN_POINT('Ctrl Pts',(20.2373980474879,-7.53962169534167,0.));
#7909=CARTESIAN_POINT('Ctrl Pts',(20.2884698940944,-7.53133155804008,0.));
#7910=CARTESIAN_POINT('Ctrl Pts',(20.3395736743243,-7.52278303006887,0.));
#7911=CARTESIAN_POINT('Ctrl Pts',(20.3907080367098,-7.51397746081994,0.));
#7912=CARTESIAN_POINT('Ctrl Pts',(20.4418717748497,-7.50491611266253,0.));
#7913=CARTESIAN_POINT('Ctrl Pts',(20.493063915616,-7.49560012018406,0.));
#7914=CARTESIAN_POINT('Ctrl Pts',(20.5545277683621,-7.48411651832413,0.));
#7915=CARTESIAN_POINT('Ctrl Pts',(20.6057817877246,-7.47423073598682,0.));
#7916=CARTESIAN_POINT('Ctrl Pts',(20.6468066077586,-7.46612041736314,0.));
#7917=CARTESIAN_POINT('Ctrl Pts',(20.6775873630604,-7.45992433946824,0.));
#7918=CARTESIAN_POINT('Ctrl Pts',(20.698113262342,-7.45574324794401,0.));
#7919=CARTESIAN_POINT('Ctrl Pts',(17.2541372868972,-7.45007618140239,13.));
#7920=CARTESIAN_POINT('Ctrl Pts',(17.2687220121489,-7.45637364573816,13.));
#7921=CARTESIAN_POINT('Ctrl Pts',(17.2834550499008,-7.46226667103919,13.));
#7922=CARTESIAN_POINT('Ctrl Pts',(17.2983267669067,-7.46778231425445,13.));
#7923=CARTESIAN_POINT('Ctrl Pts',(17.3157575315993,-7.47424706065699,13.));
#7924=CARTESIAN_POINT('Ctrl Pts',(17.3333785326113,-7.48019417753821,13.));
#7925=CARTESIAN_POINT('Ctrl Pts',(17.3511502187375,-7.48573450280811,13.));
#7926=CARTESIAN_POINT('Ctrl Pts',(17.3761558316968,-7.49353000563121,13.));
#7927=CARTESIAN_POINT('Ctrl Pts',(17.4014574303076,-7.50052692940225,13.));
#7928=CARTESIAN_POINT('Ctrl Pts',(17.4269165094415,-7.50711117101491,13.));
#7929=CARTESIAN_POINT('Ctrl Pts',(17.4438508122163,-7.51149073008789,13.));
#7930=CARTESIAN_POINT('Ctrl Pts',(17.4608540901313,-7.51568961154288,13.));
#7931=CARTESIAN_POINT('Ctrl Pts',(17.477895354957,-7.51979276933228,13.));
#7932=CARTESIAN_POINT('Ctrl Pts',(17.4958340796489,-7.52411201550939,13.));
#7933=CARTESIAN_POINT('Ctrl Pts',(17.5138146001159,-7.52832602172309,13.));
#7934=CARTESIAN_POINT('Ctrl Pts',(17.5318219263269,-7.53247314101538,13.));
#7935=CARTESIAN_POINT('Ctrl Pts',(17.5518200478141,-7.53707874400482,13.));
#7936=CARTESIAN_POINT('Ctrl Pts',(17.5718516505912,-7.54160061545737,13.));
#7937=CARTESIAN_POINT('Ctrl Pts',(17.5919190740356,-7.5460260137895,13.));
#7938=CARTESIAN_POINT('Ctrl Pts',(17.6221716888696,-7.55269751656612,13.));
#7939=CARTESIAN_POINT('Ctrl Pts',(17.6525076946371,-7.55914375118857,13.));
#7940=CARTESIAN_POINT('Ctrl Pts',(17.6829731243219,-7.56521559976811,13.));
#7941=CARTESIAN_POINT('Ctrl Pts',(17.7051055929398,-7.56962666501585,13.));
#7942=CARTESIAN_POINT('Ctrl Pts',(17.727307481075,-7.57383703867015,13.));
#7943=CARTESIAN_POINT('Ctrl Pts',(17.7495842479971,-7.57782678310872,13.));
#7944=CARTESIAN_POINT('Ctrl Pts',(17.7768156880447,-7.58270390405109,13.));
#7945=CARTESIAN_POINT('Ctrl Pts',(17.8041586050554,-7.58725254420668,13.));
#7946=CARTESIAN_POINT('Ctrl Pts',(17.8315958504975,-7.59151733245669,13.));
#7947=CARTESIAN_POINT('Ctrl Pts',(17.8612326292199,-7.59612401157578,13.));
#7948=CARTESIAN_POINT('Ctrl Pts',(17.890977551337,-7.60040516926074,13.));
#7949=CARTESIAN_POINT('Ctrl Pts',(17.9207992272247,-7.60444696777948,13.));
#7950=CARTESIAN_POINT('Ctrl Pts',(17.9483304583238,-7.60817833718655,13.));
#7951=CARTESIAN_POINT('Ctrl Pts',(17.9759263070057,-7.61170808544497,13.));
#7952=CARTESIAN_POINT('Ctrl Pts',(18.0035762489904,-7.61506270604885,13.));
#7953=CARTESIAN_POINT('Ctrl Pts',(18.0411401148466,-7.61962013038026,13.));
#7954=CARTESIAN_POINT('Ctrl Pts',(18.078804438117,-7.62385245909278,13.));
#7955=CARTESIAN_POINT('Ctrl Pts',(18.1165756810882,-7.62773031180414,13.));
#7956=CARTESIAN_POINT('Ctrl Pts',(18.1530241147805,-7.63147235591759,13.));
#7957=CARTESIAN_POINT('Ctrl Pts',(18.1895746220981,-7.63487692331431,13.));
#7958=CARTESIAN_POINT('Ctrl Pts',(18.226229844125,-7.63792794642091,13.));
#7959=CARTESIAN_POINT('Ctrl Pts',(18.2760269902476,-7.6420728467942,13.));
#7960=CARTESIAN_POINT('Ctrl Pts',(18.3260163399595,-7.64556831472346,13.));
#7961=CARTESIAN_POINT('Ctrl Pts',(18.3761647741053,-7.64849356609124,13.));
#7962=CARTESIAN_POINT('Ctrl Pts',(18.4202441575742,-7.65106479845333,13.));
#7963=CARTESIAN_POINT('Ctrl Pts',(18.4644442731323,-7.65320196597273,13.));
#7964=CARTESIAN_POINT('Ctrl Pts',(18.5087513218567,-7.65493429570881,13.));
#7965=CARTESIAN_POINT('Ctrl Pts',(18.5740706685388,-7.65748817031469,13.));
#7966=CARTESIAN_POINT('Ctrl Pts',(18.6396252901705,-7.65915358769517,13.));
#7967=CARTESIAN_POINT('Ctrl Pts',(18.7054034394317,-7.65993127489945,13.));
#7968=CARTESIAN_POINT('Ctrl Pts',(18.7884161056895,-7.66091272374024,13.));
#7969=CARTESIAN_POINT('Ctrl Pts',(18.8717830756661,-7.66048522719283,13.));
#7970=CARTESIAN_POINT('Ctrl Pts',(18.9554457129062,-7.65875983806947,13.));
#7971=CARTESIAN_POINT('Ctrl Pts',(19.0687732052289,-7.65642266547867,13.));
#7972=CARTESIAN_POINT('Ctrl Pts',(19.1826450748833,-7.65169843824266,13.));
#7973=CARTESIAN_POINT('Ctrl Pts',(19.2969757396511,-7.64469887386167,13.));
#7974=CARTESIAN_POINT('Ctrl Pts',(19.3989045212746,-7.63845857891806,13.));
#7975=CARTESIAN_POINT('Ctrl Pts',(19.5011952230427,-7.63041784747171,13.));
#7976=CARTESIAN_POINT('Ctrl Pts',(19.6037897795036,-7.62065725315813,13.));
#7977=CARTESIAN_POINT('Ctrl Pts',(19.7491944785472,-7.6068238069441,13.));
#7978=CARTESIAN_POINT('Ctrl Pts',(19.8952104286167,-7.5895301524174,13.));
#7979=CARTESIAN_POINT('Ctrl Pts',(20.0416957573265,-7.56895177464837,13.));
#7980=CARTESIAN_POINT('Ctrl Pts',(20.15548208037,-7.55296697971251,13.));
#7981=CARTESIAN_POINT('Ctrl Pts',(20.2695554921735,-7.53499708076544,13.));
#7982=CARTESIAN_POINT('Ctrl Pts',(20.3838501740658,-7.51511029118453,13.));
#7983=CARTESIAN_POINT('Ctrl Pts',(20.482723707906,-7.4979067159171,13.));
#7984=CARTESIAN_POINT('Ctrl Pts',(20.5817593863818,-7.47927116738907,13.));
#7985=CARTESIAN_POINT('Ctrl Pts',(20.6809436221336,-7.45922688157452,13.));
#7986=CARTESIAN_POINT('Ctrl Pts',(20.6866663320398,-7.45807037084351,13.));
#7987=CARTESIAN_POINT('Ctrl Pts',(20.6923895454539,-7.45690915954643,13.));
#7988=CARTESIAN_POINT('Ctrl Pts',(20.698113262342,-7.45574324794401,13.));
#7989=CARTESIAN_POINT('Ctrl Pts',(18.1978687191668,-12.3627494547115,0.));
#7990=CARTESIAN_POINT('Ctrl Pts',(18.1978687191668,-12.3627494547115,21.));
#7991=CARTESIAN_POINT('Ctrl Pts',(18.1935275957711,-12.3532177620787,0.));
#7992=CARTESIAN_POINT('Ctrl Pts',(18.1935275957711,-12.3532177620787,21.));
#7993=CARTESIAN_POINT('Ctrl Pts',(18.1848265584754,-12.3341713636489,0.));
#7994=CARTESIAN_POINT('Ctrl Pts',(18.1848265584754,-12.3341713636489,21.));
#7995=CARTESIAN_POINT('Ctrl Pts',(18.1717186310224,-12.3056527265146,0.));
#7996=CARTESIAN_POINT('Ctrl Pts',(18.1717186310224,-12.3056527265146,21.));
#7997=CARTESIAN_POINT('Ctrl Pts',(18.1541286139166,-12.2677298318549,0.));
#7998=CARTESIAN_POINT('Ctrl Pts',(18.1541286139166,-12.2677298318549,21.));
#7999=CARTESIAN_POINT('Ctrl Pts',(18.1319528884305,-12.2204964278426,0.));
#8000=CARTESIAN_POINT('Ctrl Pts',(18.1319528884305,-12.2204964278426,21.));
#8001=CARTESIAN_POINT('Ctrl Pts',(18.109588624154,-12.1734337668195,0.));
#8002=CARTESIAN_POINT('Ctrl Pts',(18.109588624154,-12.1734337668195,21.));
#8003=CARTESIAN_POINT('Ctrl Pts',(18.0870354350127,-12.1265426519718,0.));
#8004=CARTESIAN_POINT('Ctrl Pts',(18.0870354350127,-12.1265426519718,21.));
#8005=CARTESIAN_POINT('Ctrl Pts',(18.0642929289333,-12.0798241915081,0.));
#8006=CARTESIAN_POINT('Ctrl Pts',(18.0642929289333,-12.0798241915081,21.));
#8007=CARTESIAN_POINT('Ctrl Pts',(18.0413607600052,-12.0332798395991,0.));
#8008=CARTESIAN_POINT('Ctrl Pts',(18.0413607600052,-12.0332798395991,21.));
#8009=CARTESIAN_POINT('Ctrl Pts',(18.0182386160553,-11.986911314246,0.));
#8010=CARTESIAN_POINT('Ctrl Pts',(18.0182386160553,-11.986911314246,21.));
#8011=CARTESIAN_POINT('Ctrl Pts',(17.9949261997754,-11.9407205019619,0.));
#8012=CARTESIAN_POINT('Ctrl Pts',(17.9949261997754,-11.9407205019619,21.));
#8013=CARTESIAN_POINT('Ctrl Pts',(17.9714232133203,-11.8947093631895,0.));
#8014=CARTESIAN_POINT('Ctrl Pts',(17.9714232133203,-11.8947093631895,21.));
#8015=CARTESIAN_POINT('Ctrl Pts',(17.9477293432951,-11.8488798430201,0.));
#8016=CARTESIAN_POINT('Ctrl Pts',(17.9477293432951,-11.8488798430201,21.));
#8017=CARTESIAN_POINT('Ctrl Pts',(17.9238442458356,-11.8032337607271,0.));
#8018=CARTESIAN_POINT('Ctrl Pts',(17.9238442458356,-11.8032337607271,21.));
#8019=CARTESIAN_POINT('Ctrl Pts',(17.8997675418752,-11.7577728408871,0.));
#8020=CARTESIAN_POINT('Ctrl Pts',(17.8997675418752,-11.7577728408871,21.));
#8021=CARTESIAN_POINT('Ctrl Pts',(17.8754988158862,-11.7124987772363,0.));
#8022=CARTESIAN_POINT('Ctrl Pts',(17.8754988158862,-11.7124987772363,21.));
#8023=CARTESIAN_POINT('Ctrl Pts',(17.8510376144926,-11.6674132861792,0.));
#8024=CARTESIAN_POINT('Ctrl Pts',(17.8510376144926,-11.6674132861792,21.));
#8025=CARTESIAN_POINT('Ctrl Pts',(17.8263834470057,-11.6225181583564,0.));
#8026=CARTESIAN_POINT('Ctrl Pts',(17.8263834470057,-11.6225181583564,21.));
#8027=CARTESIAN_POINT('Ctrl Pts',(17.8015357852426,-11.5778153222435,0.));
#8028=CARTESIAN_POINT('Ctrl Pts',(17.8015357852426,-11.5778153222435,21.));
#8029=CARTESIAN_POINT('Ctrl Pts',(17.7764940721306,-11.5333068279912,0.));
#8030=CARTESIAN_POINT('Ctrl Pts',(17.7764940721306,-11.5333068279912,21.));
#8031=CARTESIAN_POINT('Ctrl Pts',(17.7512577332768,-11.4889948016216,0.));
#8032=CARTESIAN_POINT('Ctrl Pts',(17.7512577332768,-11.4889948016216,21.));
#8033=CARTESIAN_POINT('Ctrl Pts',(17.725826190457,-11.4448814046804,0.));
#8034=CARTESIAN_POINT('Ctrl Pts',(17.725826190457,-11.4448814046804,21.));
#8035=CARTESIAN_POINT('Ctrl Pts',(17.700198872213,-11.4009687970126,0.));
#8036=CARTESIAN_POINT('Ctrl Pts',(17.700198872213,-11.4009687970126,21.));
#8037=CARTESIAN_POINT('Ctrl Pts',(17.674375235974,-11.3572590796967,0.));
#8038=CARTESIAN_POINT('Ctrl Pts',(17.674375235974,-11.3572590796967,21.));
#8039=CARTESIAN_POINT('Ctrl Pts',(17.6483547422688,-11.3137543310722,0.));
#8040=CARTESIAN_POINT('Ctrl Pts',(17.6483547422688,-11.3137543310722,21.));
#8041=CARTESIAN_POINT('Ctrl Pts',(17.6221368072528,-11.2704566868205,0.));
#8042=CARTESIAN_POINT('Ctrl Pts',(17.6221368072528,-11.2704566868205,21.));
#8043=CARTESIAN_POINT('Ctrl Pts',(17.5957207597803,-11.2273684103052,0.));
#8044=CARTESIAN_POINT('Ctrl Pts',(17.5957207597803,-11.2273684103052,21.));
#8045=CARTESIAN_POINT('Ctrl Pts',(17.5691058058227,-11.1844919535058,0.));
#8046=CARTESIAN_POINT('Ctrl Pts',(17.5691058058227,-11.1844919535058,21.));
#8047=CARTESIAN_POINT('Ctrl Pts',(17.5422909714139,-11.1418300507683,0.));
#8048=CARTESIAN_POINT('Ctrl Pts',(17.5422909714139,-11.1418300507683,21.));
#8049=CARTESIAN_POINT('Ctrl Pts',(17.5152751467292,-11.0993856581394,0.));
#8050=CARTESIAN_POINT('Ctrl Pts',(17.5152751467292,-11.0993856581394,21.));
#8051=CARTESIAN_POINT('Ctrl Pts',(17.4880571878157,-11.0571618040371,0.));
#8052=CARTESIAN_POINT('Ctrl Pts',(17.4880571878157,-11.0571618040371,21.));
#8053=CARTESIAN_POINT('Ctrl Pts',(17.460636011184,-11.0151614525643,0.));
#8054=CARTESIAN_POINT('Ctrl Pts',(17.460636011184,-11.0151614525643,21.));
#8055=CARTESIAN_POINT('Ctrl Pts',(17.4330106728622,-10.9733873885115,0.));
#8056=CARTESIAN_POINT('Ctrl Pts',(17.4330106728622,-10.9733873885115,21.));
#8057=CARTESIAN_POINT('Ctrl Pts',(17.4051805054129,-10.9318420203801,0.));
#8058=CARTESIAN_POINT('Ctrl Pts',(17.4051805054129,-10.9318420203801,21.));
#8059=CARTESIAN_POINT('Ctrl Pts',(17.377145012528,-10.8905275295837,0.));
#8060=CARTESIAN_POINT('Ctrl Pts',(17.377145012528,-10.8905275295837,21.));
#8061=CARTESIAN_POINT('Ctrl Pts',(17.3489036079991,-10.8494462423128,0.));
#8062=CARTESIAN_POINT('Ctrl Pts',(17.3489036079991,-10.8494462423128,21.));
#8063=CARTESIAN_POINT('Ctrl Pts',(17.3204553814537,-10.8086009632423,0.));
#8064=CARTESIAN_POINT('Ctrl Pts',(17.3204553814537,-10.8086009632423,21.));
#8065=CARTESIAN_POINT('Ctrl Pts',(17.2917988998581,-10.7679952591482,0.));
#8066=CARTESIAN_POINT('Ctrl Pts',(17.2917988998581,-10.7679952591482,21.));
#8067=CARTESIAN_POINT('Ctrl Pts',(17.2629318816279,-10.7276339231608,0.));
#8068=CARTESIAN_POINT('Ctrl Pts',(17.2629318816279,-10.7276339231608,21.));
#8069=CARTESIAN_POINT('Ctrl Pts',(17.2338514174708,-10.6875226650217,0.));
#8070=CARTESIAN_POINT('Ctrl Pts',(17.2338514174708,-10.6875226650217,21.));
#8071=CARTESIAN_POINT('Ctrl Pts',(17.2045545572011,-10.6476672831754,0.));
#8072=CARTESIAN_POINT('Ctrl Pts',(17.2045545572011,-10.6476672831754,21.));
#8073=CARTESIAN_POINT('Ctrl Pts',(17.1750388395657,-10.6080729180997,0.));
#8074=CARTESIAN_POINT('Ctrl Pts',(17.1750388395657,-10.6080729180997,21.));
#8075=CARTESIAN_POINT('Ctrl Pts',(17.1453027387554,-10.5687434234512,0.));
#8076=CARTESIAN_POINT('Ctrl Pts',(17.1453027387554,-10.5687434234512,21.));
#8077=CARTESIAN_POINT('Ctrl Pts',(17.1153464189932,-10.5296803023445,0.));
#8078=CARTESIAN_POINT('Ctrl Pts',(17.1153464189932,-10.5296803023445,21.));
#8079=CARTESIAN_POINT('Ctrl Pts',(17.0851711712016,-10.4908835057575,0.));
#8080=CARTESIAN_POINT('Ctrl Pts',(17.0851711712016,-10.4908835057575,21.));
#8081=CARTESIAN_POINT('Ctrl Pts',(17.0547779975888,-10.452353435089,0.));
#8082=CARTESIAN_POINT('Ctrl Pts',(17.0547779975888,-10.452353435089,21.));
#8083=CARTESIAN_POINT('Ctrl Pts',(17.0241663361802,-10.4140927470882,0.));
#8084=CARTESIAN_POINT('Ctrl Pts',(17.0241663361802,-10.4140927470882,21.));
#8085=CARTESIAN_POINT('Ctrl Pts',(16.9933329788855,-10.3761078860454,0.));
#8086=CARTESIAN_POINT('Ctrl Pts',(16.9933329788855,-10.3761078860454,21.));
#8087=CARTESIAN_POINT('Ctrl Pts',(16.9622702798438,-10.3384116178624,0.));
#8088=CARTESIAN_POINT('Ctrl Pts',(16.9622702798438,-10.3384116178624,21.));
#8089=CARTESIAN_POINT('Ctrl Pts',(16.9309675442425,-10.3010210756062,0.));
#8090=CARTESIAN_POINT('Ctrl Pts',(16.9309675442425,-10.3010210756062,21.));
#8091=CARTESIAN_POINT('Ctrl Pts',(16.8994142530447,-10.2639532144219,0.));
#8092=CARTESIAN_POINT('Ctrl Pts',(16.8994142530447,-10.2639532144219,21.));
#8093=CARTESIAN_POINT('Ctrl Pts',(16.8676029947679,-10.2272206796636,0.));
#8094=CARTESIAN_POINT('Ctrl Pts',(16.8676029947679,-10.2272206796636,21.));
#8095=CARTESIAN_POINT('Ctrl Pts',(16.8355319435837,-10.1908283166713,0.));
#8096=CARTESIAN_POINT('Ctrl Pts',(16.8355319435837,-10.1908283166713,21.));
#8097=CARTESIAN_POINT('Ctrl Pts',(16.8032089941901,-10.1547673397274,0.));
#8098=CARTESIAN_POINT('Ctrl Pts',(16.8032089941901,-10.1547673397274,21.));
#8099=CARTESIAN_POINT('Ctrl Pts',(16.7706479198888,-10.1190207721353,0.));
#8100=CARTESIAN_POINT('Ctrl Pts',(16.7706479198888,-10.1190207721353,21.));
#8101=CARTESIAN_POINT('Ctrl Pts',(16.7378607357337,-10.0835742491038,0.));
#8102=CARTESIAN_POINT('Ctrl Pts',(16.7378607357337,-10.0835742491038,21.));
#8103=CARTESIAN_POINT('Ctrl Pts',(16.7048506904207,-10.0484259314257,0.));
#8104=CARTESIAN_POINT('Ctrl Pts',(16.7048506904207,-10.0484259314257,21.));
#8105=CARTESIAN_POINT('Ctrl Pts',(16.6716062376276,-10.0135950379525,0.));
#8106=CARTESIAN_POINT('Ctrl Pts',(16.6716062376276,-10.0135950379525,21.));
#8107=CARTESIAN_POINT('Ctrl Pts',(16.6380914029057,-9.97913546489642,0.));
#8108=CARTESIAN_POINT('Ctrl Pts',(16.6380914029057,-9.97913546489642,21.));
#8109=CARTESIAN_POINT('Ctrl Pts',(16.6042559779574,-9.94512142712911,0.));
#8110=CARTESIAN_POINT('Ctrl Pts',(16.6042559779574,-9.94512142712911,21.));
#8111=CARTESIAN_POINT('Ctrl Pts',(16.570052753238,-9.91162317616649,0.));
#8112=CARTESIAN_POINT('Ctrl Pts',(16.570052753238,-9.91162317616649,21.));
#8113=CARTESIAN_POINT('Ctrl Pts',(16.5354535643506,-9.8786843754698,0.));
#8114=CARTESIAN_POINT('Ctrl Pts',(16.5354535643506,-9.8786843754698,21.));
#8115=CARTESIAN_POINT('Ctrl Pts',(16.5004633692332,-9.84630229363522,0.));
#8116=CARTESIAN_POINT('Ctrl Pts',(16.5004633692332,-9.84630229363522,21.));
#8117=CARTESIAN_POINT('Ctrl Pts',(16.4651416449558,-9.81439757053279,0.));
#8118=CARTESIAN_POINT('Ctrl Pts',(16.4651416449558,-9.81439757053279,21.));
#8119=CARTESIAN_POINT('Ctrl Pts',(16.4295725710378,-9.78285689698058,0.));
#8120=CARTESIAN_POINT('Ctrl Pts',(16.4295725710378,-9.78285689698058,21.));
#8121=CARTESIAN_POINT('Ctrl Pts',(16.3938231282759,-9.75159288382685,0.));
#8122=CARTESIAN_POINT('Ctrl Pts',(16.3938231282759,-9.75159288382685,21.));
#8123=CARTESIAN_POINT('Ctrl Pts',(16.3579039682519,-9.72060002001012,0.));
#8124=CARTESIAN_POINT('Ctrl Pts',(16.3579039682519,-9.72060002001012,21.));
#8125=CARTESIAN_POINT('Ctrl Pts',(16.3217321000366,-9.69000797146316,0.));
#8126=CARTESIAN_POINT('Ctrl Pts',(16.3217321000366,-9.69000797146316,21.));
#8127=CARTESIAN_POINT('Ctrl Pts',(16.2850845948324,-9.66014786078746,0.));
#8128=CARTESIAN_POINT('Ctrl Pts',(16.2850845948324,-9.66014786078746,21.));
#8129=CARTESIAN_POINT('Ctrl Pts',(16.2476599387841,-9.63146315443274,0.));
#8130=CARTESIAN_POINT('Ctrl Pts',(16.2476599387841,-9.63146315443274,21.));
#8131=CARTESIAN_POINT('Ctrl Pts',(16.2168537871666,-9.60981421781524,0.));
#8132=CARTESIAN_POINT('Ctrl Pts',(16.2168537871666,-9.60981421781524,21.));
#8133=CARTESIAN_POINT('Ctrl Pts',(16.1931534965272,-9.59446643316597,0.));
#8134=CARTESIAN_POINT('Ctrl Pts',(16.1931534965272,-9.59446643316597,21.));
#8135=CARTESIAN_POINT('Ctrl Pts',(16.1770747160769,-9.58464985151483,0.));
#8136=CARTESIAN_POINT('Ctrl Pts',(16.1770747160769,-9.58464985151483,21.));
#8137=CARTESIAN_POINT('Ctrl Pts',(16.1689656784104,-9.57984538049455,0.));
#8138=CARTESIAN_POINT('Ctrl Pts',(16.1689656784104,-9.57984538049455,21.));
#8139=CARTESIAN_POINT('',(18.1978687191669,-12.3627494547114,0.));
#8140=CARTESIAN_POINT('Ctrl Pts',(16.1689656784104,-9.57984538049455,0.));
#8141=CARTESIAN_POINT('Ctrl Pts',(16.1770747160769,-9.58464985151483,0.));
#8142=CARTESIAN_POINT('Ctrl Pts',(16.1931534965272,-9.59446643316597,0.));
#8143=CARTESIAN_POINT('Ctrl Pts',(16.2168537871666,-9.60981421781524,0.));
#8144=CARTESIAN_POINT('Ctrl Pts',(16.2476599387841,-9.63146315443274,0.));
#8145=CARTESIAN_POINT('Ctrl Pts',(16.2850845948324,-9.66014786078746,0.));
#8146=CARTESIAN_POINT('Ctrl Pts',(16.3217321000366,-9.69000797146316,0.));
#8147=CARTESIAN_POINT('Ctrl Pts',(16.3579039682519,-9.72060002001012,0.));
#8148=CARTESIAN_POINT('Ctrl Pts',(16.3938231282759,-9.75159288382685,0.));
#8149=CARTESIAN_POINT('Ctrl Pts',(16.4295725710378,-9.78285689698058,0.));
#8150=CARTESIAN_POINT('Ctrl Pts',(16.4651416449558,-9.81439757053279,0.));
#8151=CARTESIAN_POINT('Ctrl Pts',(16.5004633692332,-9.84630229363522,0.));
#8152=CARTESIAN_POINT('Ctrl Pts',(16.5354535643506,-9.8786843754698,0.));
#8153=CARTESIAN_POINT('Ctrl Pts',(16.570052753238,-9.91162317616649,0.));
#8154=CARTESIAN_POINT('Ctrl Pts',(16.6042559779574,-9.94512142712911,0.));
#8155=CARTESIAN_POINT('Ctrl Pts',(16.6380914029057,-9.97913546489642,0.));
#8156=CARTESIAN_POINT('Ctrl Pts',(16.6716062376276,-10.0135950379525,0.));
#8157=CARTESIAN_POINT('Ctrl Pts',(16.7048506904207,-10.0484259314257,0.));
#8158=CARTESIAN_POINT('Ctrl Pts',(16.7378607357337,-10.0835742491038,0.));
#8159=CARTESIAN_POINT('Ctrl Pts',(16.7706479198888,-10.1190207721353,0.));
#8160=CARTESIAN_POINT('Ctrl Pts',(16.8032089941901,-10.1547673397274,0.));
#8161=CARTESIAN_POINT('Ctrl Pts',(16.8355319435837,-10.1908283166713,0.));
#8162=CARTESIAN_POINT('Ctrl Pts',(16.8676029947679,-10.2272206796636,0.));
#8163=CARTESIAN_POINT('Ctrl Pts',(16.8994142530447,-10.2639532144219,0.));
#8164=CARTESIAN_POINT('Ctrl Pts',(16.9309675442425,-10.3010210756062,0.));
#8165=CARTESIAN_POINT('Ctrl Pts',(16.9622702798438,-10.3384116178624,0.));
#8166=CARTESIAN_POINT('Ctrl Pts',(16.9933329788855,-10.3761078860454,0.));
#8167=CARTESIAN_POINT('Ctrl Pts',(17.0241663361802,-10.4140927470882,0.));
#8168=CARTESIAN_POINT('Ctrl Pts',(17.0547779975888,-10.452353435089,0.));
#8169=CARTESIAN_POINT('Ctrl Pts',(17.0851711712016,-10.4908835057575,0.));
#8170=CARTESIAN_POINT('Ctrl Pts',(17.1153464189932,-10.5296803023445,0.));
#8171=CARTESIAN_POINT('Ctrl Pts',(17.1453027387554,-10.5687434234512,0.));
#8172=CARTESIAN_POINT('Ctrl Pts',(17.1750388395657,-10.6080729180997,0.));
#8173=CARTESIAN_POINT('Ctrl Pts',(17.2045545572011,-10.6476672831754,0.));
#8174=CARTESIAN_POINT('Ctrl Pts',(17.2338514174708,-10.6875226650217,0.));
#8175=CARTESIAN_POINT('Ctrl Pts',(17.2629318816279,-10.7276339231608,0.));
#8176=CARTESIAN_POINT('Ctrl Pts',(17.2917988998581,-10.7679952591482,0.));
#8177=CARTESIAN_POINT('Ctrl Pts',(17.3204553814537,-10.8086009632423,0.));
#8178=CARTESIAN_POINT('Ctrl Pts',(17.3489036079991,-10.8494462423128,0.));
#8179=CARTESIAN_POINT('Ctrl Pts',(17.377145012528,-10.8905275295837,0.));
#8180=CARTESIAN_POINT('Ctrl Pts',(17.4051805054129,-10.9318420203801,0.));
#8181=CARTESIAN_POINT('Ctrl Pts',(17.4330106728622,-10.9733873885115,0.));
#8182=CARTESIAN_POINT('Ctrl Pts',(17.460636011184,-11.0151614525643,0.));
#8183=CARTESIAN_POINT('Ctrl Pts',(17.4880571878157,-11.0571618040371,0.));
#8184=CARTESIAN_POINT('Ctrl Pts',(17.5152751467292,-11.0993856581394,0.));
#8185=CARTESIAN_POINT('Ctrl Pts',(17.5422909714139,-11.1418300507683,0.));
#8186=CARTESIAN_POINT('Ctrl Pts',(17.5691058058227,-11.1844919535058,0.));
#8187=CARTESIAN_POINT('Ctrl Pts',(17.5957207597803,-11.2273684103052,0.));
#8188=CARTESIAN_POINT('Ctrl Pts',(17.6221368072528,-11.2704566868205,0.));
#8189=CARTESIAN_POINT('Ctrl Pts',(17.6483547422688,-11.3137543310722,0.));
#8190=CARTESIAN_POINT('Ctrl Pts',(17.674375235974,-11.3572590796967,0.));
#8191=CARTESIAN_POINT('Ctrl Pts',(17.700198872213,-11.4009687970126,0.));
#8192=CARTESIAN_POINT('Ctrl Pts',(17.725826190457,-11.4448814046804,0.));
#8193=CARTESIAN_POINT('Ctrl Pts',(17.7512577332768,-11.4889948016216,0.));
#8194=CARTESIAN_POINT('Ctrl Pts',(17.7764940721306,-11.5333068279912,0.));
#8195=CARTESIAN_POINT('Ctrl Pts',(17.8015357852426,-11.5778153222435,0.));
#8196=CARTESIAN_POINT('Ctrl Pts',(17.8263834470057,-11.6225181583564,0.));
#8197=CARTESIAN_POINT('Ctrl Pts',(17.8510376144926,-11.6674132861792,0.));
#8198=CARTESIAN_POINT('Ctrl Pts',(17.8754988158862,-11.7124987772363,0.));
#8199=CARTESIAN_POINT('Ctrl Pts',(17.8997675418752,-11.7577728408871,0.));
#8200=CARTESIAN_POINT('Ctrl Pts',(17.9238442458356,-11.8032337607271,0.));
#8201=CARTESIAN_POINT('Ctrl Pts',(17.9477293432951,-11.8488798430201,0.));
#8202=CARTESIAN_POINT('Ctrl Pts',(17.9714232133203,-11.8947093631895,0.));
#8203=CARTESIAN_POINT('Ctrl Pts',(17.9949261997754,-11.9407205019619,0.));
#8204=CARTESIAN_POINT('Ctrl Pts',(18.0182386160553,-11.986911314246,0.));
#8205=CARTESIAN_POINT('Ctrl Pts',(18.0413607600052,-12.0332798395991,0.));
#8206=CARTESIAN_POINT('Ctrl Pts',(18.0642929289333,-12.0798241915081,0.));
#8207=CARTESIAN_POINT('Ctrl Pts',(18.0870354350127,-12.1265426519718,0.));
#8208=CARTESIAN_POINT('Ctrl Pts',(18.109588624154,-12.1734337668195,0.));
#8209=CARTESIAN_POINT('Ctrl Pts',(18.1364257412858,-12.2299089600472,0.));
#8210=CARTESIAN_POINT('Ctrl Pts',(18.1585543320743,-12.2771850498068,0.));
#8211=CARTESIAN_POINT('Ctrl Pts',(18.1761067306718,-12.3151419520839,0.));
#8212=CARTESIAN_POINT('Ctrl Pts',(18.1891864723772,-12.3436860694314,0.));
#8213=CARTESIAN_POINT('Ctrl Pts',(18.1978687191668,-12.3627494547115,0.));
#8214=CARTESIAN_POINT('',(18.1978687191669,-12.3627494547114,13.));
#8215=CARTESIAN_POINT('Ctrl Pts',(18.1978687191668,-12.3627494547115,13.));
#8216=CARTESIAN_POINT('Ctrl Pts',(18.1551298837072,-12.2689088964153,13.));
#8217=CARTESIAN_POINT('Ctrl Pts',(18.1112996376559,-12.1760519707549,13.));
#8218=CARTESIAN_POINT('Ctrl Pts',(18.0663670681848,-12.0842021157222,13.));
#8219=CARTESIAN_POINT('Ctrl Pts',(17.9919118458474,-11.9320029101433,13.));
#8220=CARTESIAN_POINT('Ctrl Pts',(17.9144310030486,-11.7825824056667,13.));
#8221=CARTESIAN_POINT('Ctrl Pts',(17.8338669541097,-11.6362239749613,13.));
#8222=CARTESIAN_POINT('Ctrl Pts',(17.7719407006024,-11.5237243004517,13.));
#8223=CARTESIAN_POINT('Ctrl Pts',(17.7081904548334,-11.4130324622867,13.));
#8224=CARTESIAN_POINT('Ctrl Pts',(17.6425762040179,-11.3042990955942,13.));
#8225=CARTESIAN_POINT('Ctrl Pts',(17.5719440403086,-11.1872502401787,13.));
#8226=CARTESIAN_POINT('Ctrl Pts',(17.4991548062463,-11.0724652177424,13.));
#8227=CARTESIAN_POINT('Ctrl Pts',(17.4241207676042,-10.9601920950805,13.));
#8228=CARTESIAN_POINT('Ctrl Pts',(17.3825798893999,-10.8980346502925,13.));
#8229=CARTESIAN_POINT('Ctrl Pts',(17.3403540622895,-10.836643006144,13.));
#8230=CARTESIAN_POINT('Ctrl Pts',(17.2974271280105,-10.7760628579409,13.));
#8231=CARTESIAN_POINT('Ctrl Pts',(17.2560610445451,-10.7176854427117,13.));
#8232=CARTESIAN_POINT('Ctrl Pts',(17.2140399830246,-10.6600671042728,13.));
#8233=CARTESIAN_POINT('Ctrl Pts',(17.1713305020871,-10.6032772263326,13.));
#8234=CARTESIAN_POINT('Ctrl Pts',(17.1344164164088,-10.5541933607851,13.));
#8235=CARTESIAN_POINT('Ctrl Pts',(17.09698995673,-10.5057257117512,13.));
#8236=CARTESIAN_POINT('Ctrl Pts',(17.0590571089409,-10.4578814195699,13.));
#8237=CARTESIAN_POINT('Ctrl Pts',(17.0318344202099,-10.4235457356041,13.));
#8238=CARTESIAN_POINT('Ctrl Pts',(17.0043525707778,-10.3895287991213,13.));
#8239=CARTESIAN_POINT('Ctrl Pts',(16.9765917309458,-10.3558648806384,13.));
#8240=CARTESIAN_POINT('Ctrl Pts',(16.9492829424395,-10.3227491378977,13.));
#8241=CARTESIAN_POINT('Ctrl Pts',(16.9217004805397,-10.2899802176756,13.));
#8242=CARTESIAN_POINT('Ctrl Pts',(16.8938171690435,-10.2576030035887,13.));
#8243=CARTESIAN_POINT('Ctrl Pts',(16.8696406997029,-10.2295300566645,13.));
#8244=CARTESIAN_POINT('Ctrl Pts',(16.8452366239146,-10.2017536139349,13.));
#8245=CARTESIAN_POINT('Ctrl Pts',(16.8206160303422,-10.1742626911979,13.));
#8246=CARTESIAN_POINT('Ctrl Pts',(16.7983154207592,-10.149362221872,13.));
#8247=CARTESIAN_POINT('Ctrl Pts',(16.7758403908295,-10.1246914567643,13.));
#8248=CARTESIAN_POINT('Ctrl Pts',(16.7532063446108,-10.1002324983347,13.));
#8249=CARTESIAN_POINT('Ctrl Pts',(16.7341406199811,-10.0796295640807,13.));
#8250=CARTESIAN_POINT('Ctrl Pts',(16.7149630711762,-10.0591755007626,13.));
#8251=CARTESIAN_POINT('Ctrl Pts',(16.6956634330448,-10.0388873690432,13.));
#8252=CARTESIAN_POINT('Ctrl Pts',(16.6677347575979,-10.0095282358636,13.));
#8253=CARTESIAN_POINT('Ctrl Pts',(16.6395499069818,-9.98051721199954,13.));
#8254=CARTESIAN_POINT('Ctrl Pts',(16.6109867035167,-9.95203577348376,13.));
#8255=CARTESIAN_POINT('Ctrl Pts',(16.5937277072624,-9.93482618278573,13.));
#8256=CARTESIAN_POINT('Ctrl Pts',(16.5763285719921,-9.91781279927099,13.));
#8257=CARTESIAN_POINT('Ctrl Pts',(16.5587751448726,-9.90101792967191,13.));
#8258=CARTESIAN_POINT('Ctrl Pts',(16.5425859470632,-9.8855283352884,13.));
#8259=CARTESIAN_POINT('Ctrl Pts',(16.5262647431237,-9.87022569059541,13.));
#8260=CARTESIAN_POINT('Ctrl Pts',(16.5098269901612,-9.85509024386431,13.));
#8261=CARTESIAN_POINT('Ctrl Pts',(16.4872151945017,-9.83426990245398,13.));
#8262=CARTESIAN_POINT('Ctrl Pts',(16.4643869859048,-9.81375991308894,13.));
#8263=CARTESIAN_POINT('Ctrl Pts',(16.4414328803058,-9.79343968032572,13.));
#8264=CARTESIAN_POINT('Ctrl Pts',(16.4268703866426,-9.78054816252851,13.));
#8265=CARTESIAN_POINT('Ctrl Pts',(16.4122582104797,-9.7677316676722,13.));
#8266=CARTESIAN_POINT('Ctrl Pts',(16.3976025797345,-9.75498419487195,13.));
#8267=CARTESIAN_POINT('Ctrl Pts',(16.3844498332853,-9.74354393136336,13.));
#8268=CARTESIAN_POINT('Ctrl Pts',(16.3712625080567,-9.73215866505371,13.));
#8269=CARTESIAN_POINT('Ctrl Pts',(16.35802194704,-9.7208575105204,13.));
#8270=CARTESIAN_POINT('Ctrl Pts',(16.3441034803567,-9.70897774631286,13.));
#8271=CARTESIAN_POINT('Ctrl Pts',(16.3301262834583,-9.69719080125421,13.));
#8272=CARTESIAN_POINT('Ctrl Pts',(16.3160331240261,-9.68558166516946,13.));
#8273=CARTESIAN_POINT('Ctrl Pts',(16.2926244175233,-9.66629891592753,13.));
#8274=CARTESIAN_POINT('Ctrl Pts',(16.2688910940391,-9.6475137315389,13.));
#8275=CARTESIAN_POINT('Ctrl Pts',(16.2444806682505,-9.62974342619985,13.));
#8276=CARTESIAN_POINT('Ctrl Pts',(16.2310198906751,-9.61994424737003,13.));
#8277=CARTESIAN_POINT('Ctrl Pts',(16.2173524098891,-9.61045478087667,13.));
#8278=CARTESIAN_POINT('Ctrl Pts',(16.2034347660458,-9.60133856557799,13.));
#8279=CARTESIAN_POINT('Ctrl Pts',(16.19211348069,-9.59392299467219,13.));
#8280=CARTESIAN_POINT('Ctrl Pts',(16.1806266997874,-9.58675434325645,13.));
#8281=CARTESIAN_POINT('Ctrl Pts',(16.1689656784104,-9.57984538049455,13.));
#8282=CARTESIAN_POINT('',(18.1978687191669,-12.3627494547114,0.));
#8283=CARTESIAN_POINT('Origin',(4.58435815896522E-12,-3.3307311660966E-12,
0.));
#8284=CARTESIAN_POINT('',(17.3811241238545,-13.4869019493419,0.));
#8285=CARTESIAN_POINT('Origin',(4.58435815896522E-12,-3.3307311660966E-12,
0.));
#8286=CARTESIAN_POINT('',(17.3811241238545,-13.4869019493419,13.));
#8287=CARTESIAN_POINT('Origin',(4.58435815896522E-12,-3.3307311660966E-12,
13.));
#8288=CARTESIAN_POINT('',(17.3811241238545,-13.4869019493419,0.));
#8289=CARTESIAN_POINT('Ctrl Pts',(14.1074595503134,-12.4172651441477,0.));
#8290=CARTESIAN_POINT('Ctrl Pts',(14.1074595503134,-12.4172651441477,21.));
#8291=CARTESIAN_POINT('Ctrl Pts',(14.1145347042316,-12.4234926340671,0.));
#8292=CARTESIAN_POINT('Ctrl Pts',(14.1145347042316,-12.4234926340671,21.));
#8293=CARTESIAN_POINT('Ctrl Pts',(14.1288394445866,-12.4357509724316,0.));
#8294=CARTESIAN_POINT('Ctrl Pts',(14.1288394445866,-12.4357509724316,21.));
#8295=CARTESIAN_POINT('Ctrl Pts',(14.1507598477672,-12.4535485619997,0.));
#8296=CARTESIAN_POINT('Ctrl Pts',(14.1507598477672,-12.4535485619997,21.));
#8297=CARTESIAN_POINT('Ctrl Pts',(14.1808688343892,-12.4761570639125,0.));
#8298=CARTESIAN_POINT('Ctrl Pts',(14.1808688343892,-12.4761570639125,21.));
#8299=CARTESIAN_POINT('Ctrl Pts',(14.2197144660135,-12.5028859651751,0.));
#8300=CARTESIAN_POINT('Ctrl Pts',(14.2197144660135,-12.5028859651751,21.));
#8301=CARTESIAN_POINT('Ctrl Pts',(14.2594378207584,-12.5285125321527,0.));
#8302=CARTESIAN_POINT('Ctrl Pts',(14.2594378207584,-12.5285125321527,21.));
#8303=CARTESIAN_POINT('Ctrl Pts',(14.2997103098726,-12.5534605602317,0.));
#8304=CARTESIAN_POINT('Ctrl Pts',(14.2997103098726,-12.5534605602317,21.));
#8305=CARTESIAN_POINT('Ctrl Pts',(14.3402859058353,-12.5780443898087,0.));
#8306=CARTESIAN_POINT('Ctrl Pts',(14.3402859058353,-12.5780443898087,21.));
#8307=CARTESIAN_POINT('Ctrl Pts',(14.3810669346235,-12.6023830189244,0.));
#8308=CARTESIAN_POINT('Ctrl Pts',(14.3810669346235,-12.6023830189244,21.));
#8309=CARTESIAN_POINT('Ctrl Pts',(14.4220553460485,-12.6264646143111,0.));
#8310=CARTESIAN_POINT('Ctrl Pts',(14.4220553460485,-12.6264646143111,21.));
#8311=CARTESIAN_POINT('Ctrl Pts',(14.463313553928,-12.6501984687124,0.));
#8312=CARTESIAN_POINT('Ctrl Pts',(14.463313553928,-12.6501984687124,21.));
#8313=CARTESIAN_POINT('Ctrl Pts',(14.5049233087958,-12.6734695081852,0.));
#8314=CARTESIAN_POINT('Ctrl Pts',(14.5049233087958,-12.6734695081852,21.));
#8315=CARTESIAN_POINT('Ctrl Pts',(14.5469417071951,-12.6961966430455,0.));
#8316=CARTESIAN_POINT('Ctrl Pts',(14.5469417071951,-12.6961966430455,21.));
#8317=CARTESIAN_POINT('Ctrl Pts',(14.5893698147583,-12.7183743139638,0.));
#8318=CARTESIAN_POINT('Ctrl Pts',(14.5893698147583,-12.7183743139638,21.));
#8319=CARTESIAN_POINT('Ctrl Pts',(14.6321748083434,-12.7400427996252,0.));
#8320=CARTESIAN_POINT('Ctrl Pts',(14.6321748083434,-12.7400427996252,21.));
#8321=CARTESIAN_POINT('Ctrl Pts',(14.6753044633399,-12.7612687078867,0.));
#8322=CARTESIAN_POINT('Ctrl Pts',(14.6753044633399,-12.7612687078867,21.));
#8323=CARTESIAN_POINT('Ctrl Pts',(14.7187037124277,-12.7821227233337,0.));
#8324=CARTESIAN_POINT('Ctrl Pts',(14.7187037124277,-12.7821227233337,21.));
#8325=CARTESIAN_POINT('Ctrl Pts',(14.7623324139791,-12.8026557145457,0.));
#8326=CARTESIAN_POINT('Ctrl Pts',(14.7623324139791,-12.8026557145457,21.));
#8327=CARTESIAN_POINT('Ctrl Pts',(14.8061758577898,-12.8228846016791,0.));
#8328=CARTESIAN_POINT('Ctrl Pts',(14.8061758577898,-12.8228846016791,21.));
#8329=CARTESIAN_POINT('Ctrl Pts',(14.8502347891476,-12.8428057266944,0.));
#8330=CARTESIAN_POINT('Ctrl Pts',(14.8502347891476,-12.8428057266944,21.));
#8331=CARTESIAN_POINT('Ctrl Pts',(14.8945191569251,-12.8624032236317,0.));
#8332=CARTESIAN_POINT('Ctrl Pts',(14.8945191569251,-12.8624032236317,21.));
#8333=CARTESIAN_POINT('Ctrl Pts',(14.9390408507356,-12.8816587472148,0.));
#8334=CARTESIAN_POINT('Ctrl Pts',(14.9390408507356,-12.8816587472148,21.));
#8335=CARTESIAN_POINT('Ctrl Pts',(14.9838057866976,-12.9005620742036,0.));
#8336=CARTESIAN_POINT('Ctrl Pts',(14.9838057866976,-12.9005620742036,21.));
#8337=CARTESIAN_POINT('Ctrl Pts',(15.0288099208306,-12.9191164383568,0.));
#8338=CARTESIAN_POINT('Ctrl Pts',(15.0288099208306,-12.9191164383568,21.));
#8339=CARTESIAN_POINT('Ctrl Pts',(15.0740435169624,-12.9373327960422,0.));
#8340=CARTESIAN_POINT('Ctrl Pts',(15.0740435169624,-12.9373327960422,21.));
#8341=CARTESIAN_POINT('Ctrl Pts',(15.1194937003528,-12.9552263908864,0.));
#8342=CARTESIAN_POINT('Ctrl Pts',(15.1194937003528,-12.9552263908864,21.));
#8343=CARTESIAN_POINT('Ctrl Pts',(15.1651474813659,-12.9728126886697,0.));
#8344=CARTESIAN_POINT('Ctrl Pts',(15.1651474813659,-12.9728126886697,21.));
#8345=CARTESIAN_POINT('Ctrl Pts',(15.2109950816083,-12.9901029059182,0.));
#8346=CARTESIAN_POINT('Ctrl Pts',(15.2109950816083,-12.9901029059182,21.));
#8347=CARTESIAN_POINT('Ctrl Pts',(15.2570313635503,-13.0071020851025,0.));
#8348=CARTESIAN_POINT('Ctrl Pts',(15.2570313635503,-13.0071020851025,21.));
#8349=CARTESIAN_POINT('Ctrl Pts',(15.3032539741328,-13.0238115816729,0.));
#8350=CARTESIAN_POINT('Ctrl Pts',(15.3032539741328,-13.0238115816729,21.));
#8351=CARTESIAN_POINT('Ctrl Pts',(15.3496622219036,-13.0402305665115,0.));
#8352=CARTESIAN_POINT('Ctrl Pts',(15.3496622219036,-13.0402305665115,21.));
#8353=CARTESIAN_POINT('Ctrl Pts',(15.3962557545684,-13.0563577967298,0.));
#8354=CARTESIAN_POINT('Ctrl Pts',(15.3962557545684,-13.0563577967298,21.));
#8355=CARTESIAN_POINT('Ctrl Pts',(15.4430330918328,-13.0721935806302,0.));
#8356=CARTESIAN_POINT('Ctrl Pts',(15.4430330918328,-13.0721935806302,21.));
#8357=CARTESIAN_POINT('Ctrl Pts',(15.4899910401523,-13.087740560189,0.));
#8358=CARTESIAN_POINT('Ctrl Pts',(15.4899910401523,-13.087740560189,21.));
#8359=CARTESIAN_POINT('Ctrl Pts',(15.5371254712111,-13.1030026646917,0.));
#8360=CARTESIAN_POINT('Ctrl Pts',(15.5371254712111,-13.1030026646917,21.));
#8361=CARTESIAN_POINT('Ctrl Pts',(15.5844317820184,-13.1179844917497,0.));
#8362=CARTESIAN_POINT('Ctrl Pts',(15.5844317820184,-13.1179844917497,21.));
#8363=CARTESIAN_POINT('Ctrl Pts',(15.6319054413079,-13.1326905726717,0.));
#8364=CARTESIAN_POINT('Ctrl Pts',(15.6319054413079,-13.1326905726717,21.));
#8365=CARTESIAN_POINT('Ctrl Pts',(15.6795425955901,-13.147124558532,0.));
#8366=CARTESIAN_POINT('Ctrl Pts',(15.6795425955901,-13.147124558532,21.));
#8367=CARTESIAN_POINT('Ctrl Pts',(15.7273402954914,-13.161288914421,0.));
#8368=CARTESIAN_POINT('Ctrl Pts',(15.7273402954914,-13.161288914421,21.));
#8369=CARTESIAN_POINT('Ctrl Pts',(15.7752961549278,-13.1751853728467,0.));
#8370=CARTESIAN_POINT('Ctrl Pts',(15.7752961549278,-13.1751853728467,21.));
#8371=CARTESIAN_POINT('Ctrl Pts',(15.8234081427091,-13.1888152101588,0.));
#8372=CARTESIAN_POINT('Ctrl Pts',(15.8234081427091,-13.1888152101588,21.));
#8373=CARTESIAN_POINT('Ctrl Pts',(15.8716743375555,-13.2021795724682,0.));
#8374=CARTESIAN_POINT('Ctrl Pts',(15.8716743375555,-13.2021795724682,21.));
#8375=CARTESIAN_POINT('Ctrl Pts',(15.9200926550954,-13.2152798388134,0.));
#8376=CARTESIAN_POINT('Ctrl Pts',(15.9200926550954,-13.2152798388134,21.));
#8377=CARTESIAN_POINT('Ctrl Pts',(15.9686607385389,-13.2281177675127,0.));
#8378=CARTESIAN_POINT('Ctrl Pts',(15.9686607385389,-13.2281177675127,21.));
#8379=CARTESIAN_POINT('Ctrl Pts',(16.0173761036734,-13.240695304984,0.));
#8380=CARTESIAN_POINT('Ctrl Pts',(16.0173761036734,-13.240695304984,21.));
#8381=CARTESIAN_POINT('Ctrl Pts',(16.0662362238032,-13.2530144750236,0.));
#8382=CARTESIAN_POINT('Ctrl Pts',(16.0662362238032,-13.2530144750236,21.));
#8383=CARTESIAN_POINT('Ctrl Pts',(16.1152386305152,-13.2650772466062,0.));
#8384=CARTESIAN_POINT('Ctrl Pts',(16.1152386305152,-13.2650772466062,21.));
#8385=CARTESIAN_POINT('Ctrl Pts',(16.1643810242643,-13.2768853909882,0.));
#8386=CARTESIAN_POINT('Ctrl Pts',(16.1643810242643,-13.2768853909882,21.));
#8387=CARTESIAN_POINT('Ctrl Pts',(16.2136613184475,-13.2884404210388,0.));
#8388=CARTESIAN_POINT('Ctrl Pts',(16.2136613184475,-13.2884404210388,21.));
#8389=CARTESIAN_POINT('Ctrl Pts',(16.2630775678735,-13.2997436744733,0.));
#8390=CARTESIAN_POINT('Ctrl Pts',(16.2630775678735,-13.2997436744733,21.));
#8391=CARTESIAN_POINT('Ctrl Pts',(16.3126279218067,-13.3107963665229,0.));
#8392=CARTESIAN_POINT('Ctrl Pts',(16.3126279218067,-13.3107963665229,21.));
#8393=CARTESIAN_POINT('Ctrl Pts',(16.3623105703343,-13.3215996524974,0.));
#8394=CARTESIAN_POINT('Ctrl Pts',(16.3623105703343,-13.3215996524974,21.));
#8395=CARTESIAN_POINT('Ctrl Pts',(16.4121236828756,-13.3321546976812,0.));
#8396=CARTESIAN_POINT('Ctrl Pts',(16.4121236828756,-13.3321546976812,21.));
#8397=CARTESIAN_POINT('Ctrl Pts',(16.4620653818862,-13.3424627129921,0.));
#8398=CARTESIAN_POINT('Ctrl Pts',(16.4620653818862,-13.3424627129921,21.));
#8399=CARTESIAN_POINT('Ctrl Pts',(16.5121337902953,-13.3525249163084,0.));
#8400=CARTESIAN_POINT('Ctrl Pts',(16.5121337902953,-13.3525249163084,21.));
#8401=CARTESIAN_POINT('Ctrl Pts',(16.5623270636327,-13.3623425108873,0.));
#8402=CARTESIAN_POINT('Ctrl Pts',(16.5623270636327,-13.3623425108873,21.));
#8403=CARTESIAN_POINT('Ctrl Pts',(16.612643424234,-13.3719166600676,0.));
#8404=CARTESIAN_POINT('Ctrl Pts',(16.612643424234,-13.3719166600676,21.));
#8405=CARTESIAN_POINT('Ctrl Pts',(16.6630812012276,-13.3812484621131,0.));
#8406=CARTESIAN_POINT('Ctrl Pts',(16.6630812012276,-13.3812484621131,21.));
#8407=CARTESIAN_POINT('Ctrl Pts',(16.7136388432444,-13.3903389370346,0.));
#8408=CARTESIAN_POINT('Ctrl Pts',(16.7136388432444,-13.3903389370346,21.));
#8409=CARTESIAN_POINT('Ctrl Pts',(16.7643148579872,-13.3991890464165,0.));
#8410=CARTESIAN_POINT('Ctrl Pts',(16.7643148579872,-13.3991890464165,21.));
#8411=CARTESIAN_POINT('Ctrl Pts',(16.8151077630226,-13.4077997088426,0.));
#8412=CARTESIAN_POINT('Ctrl Pts',(16.8151077630226,-13.4077997088426,21.));
#8413=CARTESIAN_POINT('Ctrl Pts',(16.8660160353187,-13.4161718177499,0.));
#8414=CARTESIAN_POINT('Ctrl Pts',(16.8660160353187,-13.4161718177499,21.));
#8415=CARTESIAN_POINT('Ctrl Pts',(16.9170380509036,-13.4243062623592,0.));
#8416=CARTESIAN_POINT('Ctrl Pts',(16.9170380509036,-13.4243062623592,21.));
#8417=CARTESIAN_POINT('Ctrl Pts',(16.9681720567298,-13.432203941793,0.));
#8418=CARTESIAN_POINT('Ctrl Pts',(16.9681720567298,-13.432203941793,21.));
#8419=CARTESIAN_POINT('Ctrl Pts',(17.0194162803447,-13.4398657451291,0.));
#8420=CARTESIAN_POINT('Ctrl Pts',(17.0194162803447,-13.4398657451291,21.));
#8421=CARTESIAN_POINT('Ctrl Pts',(17.0707690194411,-13.4472925380889,0.));
#8422=CARTESIAN_POINT('Ctrl Pts',(17.0707690194411,-13.4472925380889,21.));
#8423=CARTESIAN_POINT('Ctrl Pts',(17.1222287365697,-13.4544851484583,0.));
#8424=CARTESIAN_POINT('Ctrl Pts',(17.1222287365697,-13.4544851484583,21.));
#8425=CARTESIAN_POINT('Ctrl Pts',(17.1737941556239,-13.4614443545811,0.));
#8426=CARTESIAN_POINT('Ctrl Pts',(17.1737941556239,-13.4614443545811,21.));
#8427=CARTESIAN_POINT('Ctrl Pts',(17.2254643437923,-13.4681708717969,0.));
#8428=CARTESIAN_POINT('Ctrl Pts',(17.2254643437923,-13.4681708717969,21.));
#8429=CARTESIAN_POINT('Ctrl Pts',(17.2772386565028,-13.474665315482,0.));
#8430=CARTESIAN_POINT('Ctrl Pts',(17.2772386565028,-13.474665315482,21.));
#8431=CARTESIAN_POINT('Ctrl Pts',(17.3187410868027,-13.4796755969465,0.));
#8432=CARTESIAN_POINT('Ctrl Pts',(17.3187410868027,-13.4796755969465,21.));
#8433=CARTESIAN_POINT('Ctrl Pts',(17.3499144948292,-13.4833292332349,0.));
#8434=CARTESIAN_POINT('Ctrl Pts',(17.3499144948292,-13.4833292332349,21.));
#8435=CARTESIAN_POINT('Ctrl Pts',(17.3707174645609,-13.485718750657,0.));
#8436=CARTESIAN_POINT('Ctrl Pts',(17.3707174645609,-13.485718750657,21.));
#8437=CARTESIAN_POINT('Ctrl Pts',(17.3811241238545,-13.4869019493419,0.));
#8438=CARTESIAN_POINT('Ctrl Pts',(17.3811241238545,-13.4869019493419,21.));
#8439=CARTESIAN_POINT('Ctrl Pts',(14.1074595503134,-12.4172651441477,0.));
#8440=CARTESIAN_POINT('Ctrl Pts',(14.1145347042316,-12.4234926340671,0.));
#8441=CARTESIAN_POINT('Ctrl Pts',(14.1288394445866,-12.4357509724316,0.));
#8442=CARTESIAN_POINT('Ctrl Pts',(14.1507598477672,-12.4535485619997,0.));
#8443=CARTESIAN_POINT('Ctrl Pts',(14.1808688343892,-12.4761570639125,0.));
#8444=CARTESIAN_POINT('Ctrl Pts',(14.2197144660135,-12.5028859651751,0.));
#8445=CARTESIAN_POINT('Ctrl Pts',(14.2594378207584,-12.5285125321527,0.));
#8446=CARTESIAN_POINT('Ctrl Pts',(14.2997103098726,-12.5534605602317,0.));
#8447=CARTESIAN_POINT('Ctrl Pts',(14.3402859058353,-12.5780443898087,0.));
#8448=CARTESIAN_POINT('Ctrl Pts',(14.3810669346235,-12.6023830189244,0.));
#8449=CARTESIAN_POINT('Ctrl Pts',(14.4220553460485,-12.6264646143111,0.));
#8450=CARTESIAN_POINT('Ctrl Pts',(14.463313553928,-12.6501984687124,0.));
#8451=CARTESIAN_POINT('Ctrl Pts',(14.5049233087958,-12.6734695081852,0.));
#8452=CARTESIAN_POINT('Ctrl Pts',(14.5469417071951,-12.6961966430455,0.));
#8453=CARTESIAN_POINT('Ctrl Pts',(14.5893698147583,-12.7183743139638,0.));
#8454=CARTESIAN_POINT('Ctrl Pts',(14.6321748083434,-12.7400427996252,0.));
#8455=CARTESIAN_POINT('Ctrl Pts',(14.6753044633399,-12.7612687078867,0.));
#8456=CARTESIAN_POINT('Ctrl Pts',(14.7187037124277,-12.7821227233337,0.));
#8457=CARTESIAN_POINT('Ctrl Pts',(14.7623324139791,-12.8026557145457,0.));
#8458=CARTESIAN_POINT('Ctrl Pts',(14.8061758577898,-12.8228846016791,0.));
#8459=CARTESIAN_POINT('Ctrl Pts',(14.8502347891476,-12.8428057266944,0.));
#8460=CARTESIAN_POINT('Ctrl Pts',(14.8945191569251,-12.8624032236317,0.));
#8461=CARTESIAN_POINT('Ctrl Pts',(14.9390408507356,-12.8816587472148,0.));
#8462=CARTESIAN_POINT('Ctrl Pts',(14.9838057866976,-12.9005620742036,0.));
#8463=CARTESIAN_POINT('Ctrl Pts',(15.0288099208306,-12.9191164383568,0.));
#8464=CARTESIAN_POINT('Ctrl Pts',(15.0740435169624,-12.9373327960422,0.));
#8465=CARTESIAN_POINT('Ctrl Pts',(15.1194937003528,-12.9552263908864,0.));
#8466=CARTESIAN_POINT('Ctrl Pts',(15.1651474813659,-12.9728126886697,0.));
#8467=CARTESIAN_POINT('Ctrl Pts',(15.2109950816083,-12.9901029059182,0.));
#8468=CARTESIAN_POINT('Ctrl Pts',(15.2570313635503,-13.0071020851025,0.));
#8469=CARTESIAN_POINT('Ctrl Pts',(15.3032539741328,-13.0238115816729,0.));
#8470=CARTESIAN_POINT('Ctrl Pts',(15.3496622219036,-13.0402305665115,0.));
#8471=CARTESIAN_POINT('Ctrl Pts',(15.3962557545684,-13.0563577967298,0.));
#8472=CARTESIAN_POINT('Ctrl Pts',(15.4430330918328,-13.0721935806302,0.));
#8473=CARTESIAN_POINT('Ctrl Pts',(15.4899910401523,-13.087740560189,0.));
#8474=CARTESIAN_POINT('Ctrl Pts',(15.5371254712111,-13.1030026646917,0.));
#8475=CARTESIAN_POINT('Ctrl Pts',(15.5844317820184,-13.1179844917497,0.));
#8476=CARTESIAN_POINT('Ctrl Pts',(15.6319054413079,-13.1326905726717,0.));
#8477=CARTESIAN_POINT('Ctrl Pts',(15.6795425955901,-13.147124558532,0.));
#8478=CARTESIAN_POINT('Ctrl Pts',(15.7273402954914,-13.161288914421,0.));
#8479=CARTESIAN_POINT('Ctrl Pts',(15.7752961549278,-13.1751853728467,0.));
#8480=CARTESIAN_POINT('Ctrl Pts',(15.8234081427091,-13.1888152101588,0.));
#8481=CARTESIAN_POINT('Ctrl Pts',(15.8716743375555,-13.2021795724682,0.));
#8482=CARTESIAN_POINT('Ctrl Pts',(15.9200926550954,-13.2152798388134,0.));
#8483=CARTESIAN_POINT('Ctrl Pts',(15.9686607385389,-13.2281177675127,0.));
#8484=CARTESIAN_POINT('Ctrl Pts',(16.0173761036734,-13.240695304984,0.));
#8485=CARTESIAN_POINT('Ctrl Pts',(16.0662362238032,-13.2530144750236,0.));
#8486=CARTESIAN_POINT('Ctrl Pts',(16.1152386305152,-13.2650772466062,0.));
#8487=CARTESIAN_POINT('Ctrl Pts',(16.1643810242643,-13.2768853909882,0.));
#8488=CARTESIAN_POINT('Ctrl Pts',(16.2136613184475,-13.2884404210388,0.));
#8489=CARTESIAN_POINT('Ctrl Pts',(16.2630775678735,-13.2997436744733,0.));
#8490=CARTESIAN_POINT('Ctrl Pts',(16.3126279218067,-13.3107963665229,0.));
#8491=CARTESIAN_POINT('Ctrl Pts',(16.3623105703343,-13.3215996524974,0.));
#8492=CARTESIAN_POINT('Ctrl Pts',(16.4121236828756,-13.3321546976812,0.));
#8493=CARTESIAN_POINT('Ctrl Pts',(16.4620653818862,-13.3424627129921,0.));
#8494=CARTESIAN_POINT('Ctrl Pts',(16.5121337902953,-13.3525249163084,0.));
#8495=CARTESIAN_POINT('Ctrl Pts',(16.5623270636327,-13.3623425108873,0.));
#8496=CARTESIAN_POINT('Ctrl Pts',(16.612643424234,-13.3719166600676,0.));
#8497=CARTESIAN_POINT('Ctrl Pts',(16.6630812012276,-13.3812484621131,0.));
#8498=CARTESIAN_POINT('Ctrl Pts',(16.7136388432444,-13.3903389370346,0.));
#8499=CARTESIAN_POINT('Ctrl Pts',(16.7643148579872,-13.3991890464165,0.));
#8500=CARTESIAN_POINT('Ctrl Pts',(16.8151077630226,-13.4077997088426,0.));
#8501=CARTESIAN_POINT('Ctrl Pts',(16.8660160353187,-13.4161718177499,0.));
#8502=CARTESIAN_POINT('Ctrl Pts',(16.9170380509036,-13.4243062623592,0.));
#8503=CARTESIAN_POINT('Ctrl Pts',(16.9681720567298,-13.432203941793,0.));
#8504=CARTESIAN_POINT('Ctrl Pts',(17.0194162803447,-13.4398657451291,0.));
#8505=CARTESIAN_POINT('Ctrl Pts',(17.0707690194411,-13.4472925380889,0.));
#8506=CARTESIAN_POINT('Ctrl Pts',(17.1222287365697,-13.4544851484583,0.));
#8507=CARTESIAN_POINT('Ctrl Pts',(17.1737941556239,-13.4614443545811,0.));
#8508=CARTESIAN_POINT('Ctrl Pts',(17.235798381426,-13.4695161752401,0.));
#8509=CARTESIAN_POINT('Ctrl Pts',(17.287598725272,-13.4759526005425,0.));
#8510=CARTESIAN_POINT('Ctrl Pts',(17.3291218739796,-13.4809165957478,0.));
#8511=CARTESIAN_POINT('Ctrl Pts',(17.360310805254,-13.4845355519784,0.));
#8512=CARTESIAN_POINT('Ctrl Pts',(17.3811241238545,-13.4869019493419,0.));
#8513=CARTESIAN_POINT('Ctrl Pts',(14.1074595503134,-12.4172651441477,13.));
#8514=CARTESIAN_POINT('Ctrl Pts',(14.1180860484761,-12.4266184968736,13.));
#8515=CARTESIAN_POINT('Ctrl Pts',(14.1292464564073,-12.4359861199749,13.));
#8516=CARTESIAN_POINT('Ctrl Pts',(14.1409284550598,-12.445307812124,13.));
#8517=CARTESIAN_POINT('Ctrl Pts',(14.1528807347634,-12.4548451759939,13.));
#8518=CARTESIAN_POINT('Ctrl Pts',(14.1653792068345,-12.4643342258775,13.));
#8519=CARTESIAN_POINT('Ctrl Pts',(14.1783758854621,-12.4737554908686,13.));
#8520=CARTESIAN_POINT('Ctrl Pts',(14.1924534932842,-12.4839603191584,13.));
#8521=CARTESIAN_POINT('Ctrl Pts',(14.2071153071741,-12.4940860551492,13.));
#8522=CARTESIAN_POINT('Ctrl Pts',(14.2222596346423,-12.5041603567402,13.));
#8523=CARTESIAN_POINT('Ctrl Pts',(14.2425470972603,-12.5176559720034,13.));
#8524=CARTESIAN_POINT('Ctrl Pts',(14.263696154001,-12.5310650489192,13.));
#8525=CARTESIAN_POINT('Ctrl Pts',(14.2854153020687,-12.5445127338131,13.));
#8526=CARTESIAN_POINT('Ctrl Pts',(14.3006710264832,-12.5539585083028,13.));
#8527=CARTESIAN_POINT('Ctrl Pts',(14.3162064779772,-12.5634252742744,13.));
#8528=CARTESIAN_POINT('Ctrl Pts',(14.3319443081693,-12.5729244441011,13.));
#8529=CARTESIAN_POINT('Ctrl Pts',(14.3490377565112,-12.5832418491526,13.));
#8530=CARTESIAN_POINT('Ctrl Pts',(14.3663701856948,-12.5935971521702,13.));
#8531=CARTESIAN_POINT('Ctrl Pts',(14.3838818725371,-12.603952675227,13.));
#8532=CARTESIAN_POINT('Ctrl Pts',(14.4097088777849,-12.6192254556702,13.));
#8533=CARTESIAN_POINT('Ctrl Pts',(14.4359272218094,-12.6344967052057,13.));
#8534=CARTESIAN_POINT('Ctrl Pts',(14.4624310404448,-12.6495328172899,13.));
#8535=CARTESIAN_POINT('Ctrl Pts',(14.4814589433508,-12.6603277025386,13.));
#8536=CARTESIAN_POINT('Ctrl Pts',(14.50063705981,-12.6709973404779,13.));
#8537=CARTESIAN_POINT('Ctrl Pts',(14.5199130488615,-12.6814735010565,13.));
#8538=CARTESIAN_POINT('Ctrl Pts',(14.5408480305397,-12.6928512949111,13.));
#8539=CARTESIAN_POINT('Ctrl Pts',(14.561898127647,-12.7040013081349,13.));
#8540=CARTESIAN_POINT('Ctrl Pts',(14.5829561351059,-12.7148903419541,13.));
#8541=CARTESIAN_POINT('Ctrl Pts',(14.6211007133001,-12.7346147913249,13.));
#8542=CARTESIAN_POINT('Ctrl Pts',(14.6592670224042,-12.7534882591773,13.));
#8543=CARTESIAN_POINT('Ctrl Pts',(14.6966913606211,-12.7714870012811,13.));
#8544=CARTESIAN_POINT('Ctrl Pts',(14.7236044494553,-12.7844304965631,13.));
#8545=CARTESIAN_POINT('Ctrl Pts',(14.7501320324422,-12.7969241359761,13.));
#8546=CARTESIAN_POINT('Ctrl Pts',(14.7760241380399,-12.8089152121945,13.));
#8547=CARTESIAN_POINT('Ctrl Pts',(14.79015789262,-12.815460795279,13.));
#8548=CARTESIAN_POINT('Ctrl Pts',(14.804103015233,-12.8218556822256,13.));
#8549=CARTESIAN_POINT('Ctrl Pts',(14.817821671297,-12.8280877109818,13.));
#8550=CARTESIAN_POINT('Ctrl Pts',(14.8203721510302,-12.8292463276105,13.));
#8551=CARTESIAN_POINT('Ctrl Pts',(14.8229148051886,-12.8303993130268,13.));
#8552=CARTESIAN_POINT('Ctrl Pts',(14.8254493925092,-12.8315465871292,13.));
#8553=CARTESIAN_POINT('Ctrl Pts',(14.8277305341092,-12.832579139711,13.));
#8554=CARTESIAN_POINT('Ctrl Pts',(14.8300032273041,-12.8336062098177,13.));
#8555=CARTESIAN_POINT('Ctrl Pts',(14.8322881977108,-12.8346371473846,13.));
#8556=CARTESIAN_POINT('Ctrl Pts',(14.8691293241314,-12.8512592012736,13.));
#8557=CARTESIAN_POINT('Ctrl Pts',(14.9079857431047,-12.8683541689141,13.));
#8558=CARTESIAN_POINT('Ctrl Pts',(14.9490190997324,-12.8857980615984,13.));
#8559=CARTESIAN_POINT('Ctrl Pts',(14.9855964769819,-12.9013476509045,13.));
#8560=CARTESIAN_POINT('Ctrl Pts',(15.0239050647886,-12.9171725830662,13.));
#8561=CARTESIAN_POINT('Ctrl Pts',(15.064023510322,-12.9332300933654,13.));
#8562=CARTESIAN_POINT('Ctrl Pts',(15.1048519750733,-12.9495717906701,13.));
#8563=CARTESIAN_POINT('Ctrl Pts',(15.1475508470956,-12.9661598906376,13.));
#8564=CARTESIAN_POINT('Ctrl Pts',(15.1921895453309,-12.9829638510743,13.));
#8565=CARTESIAN_POINT('Ctrl Pts',(15.2412011844821,-13.0014139779327,13.));
#8566=CARTESIAN_POINT('Ctrl Pts',(15.2925510989723,-13.0201247782342,13.));
#8567=CARTESIAN_POINT('Ctrl Pts',(15.346375635884,-13.0389903700256,13.));
#8568=CARTESIAN_POINT('Ctrl Pts',(15.4033983407683,-13.0589769251344,13.));
#8569=CARTESIAN_POINT('Ctrl Pts',(15.463204290969,-13.0791295844046,13.));
#8570=CARTESIAN_POINT('Ctrl Pts',(15.5259445689097,-13.0993286205218,13.));
#8571=CARTESIAN_POINT('Ctrl Pts',(15.5603875849943,-13.1104174417498,13.));
#8572=CARTESIAN_POINT('Ctrl Pts',(15.5957139525594,-13.1215213991741,13.));
#8573=CARTESIAN_POINT('Ctrl Pts',(15.6319463225903,-13.1326225390231,13.));
#8574=CARTESIAN_POINT('Ctrl Pts',(15.7414124455009,-13.1661615743695,13.));
#8575=CARTESIAN_POINT('Ctrl Pts',(15.8520448442677,-13.1975021501202,13.));
#8576=CARTESIAN_POINT('Ctrl Pts',(15.9635479480078,-13.2267056266809,13.));
#8577=CARTESIAN_POINT('Ctrl Pts',(16.0693084576609,-13.2544050759436,13.));
#8578=CARTESIAN_POINT('Ctrl Pts',(16.1758473117503,-13.2801884271853,13.));
#8579=CARTESIAN_POINT('Ctrl Pts',(16.2829053991411,-13.3041300678694,13.));
#8580=CARTESIAN_POINT('Ctrl Pts',(16.4340206583829,-13.337924312908,13.));
#8581=CARTESIAN_POINT('Ctrl Pts',(16.5861745378189,-13.3680402223278,13.));
#8582=CARTESIAN_POINT('Ctrl Pts',(16.7386734005371,-13.394678434022,13.));
#8583=CARTESIAN_POINT('Ctrl Pts',(16.8568706863481,-13.415324911412,13.));
#8584=CARTESIAN_POINT('Ctrl Pts',(16.9752796560061,-13.4338812595667,13.));
#8585=CARTESIAN_POINT('Ctrl Pts',(17.0935769510192,-13.4504489425771,13.));
#8586=CARTESIAN_POINT('Ctrl Pts',(17.1895488140305,-13.4638899211228,13.));
#8587=CARTESIAN_POINT('Ctrl Pts',(17.2854448391807,-13.4760235684317,13.));
#8588=CARTESIAN_POINT('Ctrl Pts',(17.3811241238545,-13.4869019493419,13.));
#8589=CARTESIAN_POINT('Ctrl Pts',(13.4869019493419,-17.3811241238545,0.));
#8590=CARTESIAN_POINT('Ctrl Pts',(13.4869019493419,-17.3811241238545,21.));
#8591=CARTESIAN_POINT('Ctrl Pts',(13.485718750657,-17.3707174645609,0.));
#8592=CARTESIAN_POINT('Ctrl Pts',(13.485718750657,-17.3707174645609,21.));
#8593=CARTESIAN_POINT('Ctrl Pts',(13.4833292332349,-17.3499144948292,0.));
#8594=CARTESIAN_POINT('Ctrl Pts',(13.4833292332349,-17.3499144948292,21.));
#8595=CARTESIAN_POINT('Ctrl Pts',(13.4796755969465,-17.3187410868027,0.));
#8596=CARTESIAN_POINT('Ctrl Pts',(13.4796755969465,-17.3187410868027,21.));
#8597=CARTESIAN_POINT('Ctrl Pts',(13.474665315482,-17.2772386565028,0.));
#8598=CARTESIAN_POINT('Ctrl Pts',(13.474665315482,-17.2772386565028,21.));
#8599=CARTESIAN_POINT('Ctrl Pts',(13.4681708717968,-17.2254643437923,0.));
#8600=CARTESIAN_POINT('Ctrl Pts',(13.4681708717968,-17.2254643437923,21.));
#8601=CARTESIAN_POINT('Ctrl Pts',(13.4614443545811,-17.173794155624,0.));
#8602=CARTESIAN_POINT('Ctrl Pts',(13.4614443545811,-17.173794155624,21.));
#8603=CARTESIAN_POINT('Ctrl Pts',(13.4544851484583,-17.1222287365697,0.));
#8604=CARTESIAN_POINT('Ctrl Pts',(13.4544851484583,-17.1222287365697,21.));
#8605=CARTESIAN_POINT('Ctrl Pts',(13.4472925380889,-17.0707690194412,0.));
#8606=CARTESIAN_POINT('Ctrl Pts',(13.4472925380889,-17.0707690194412,21.));
#8607=CARTESIAN_POINT('Ctrl Pts',(13.4398657451291,-17.0194162803447,0.));
#8608=CARTESIAN_POINT('Ctrl Pts',(13.4398657451291,-17.0194162803447,21.));
#8609=CARTESIAN_POINT('Ctrl Pts',(13.432203941793,-16.9681720567298,0.));
#8610=CARTESIAN_POINT('Ctrl Pts',(13.432203941793,-16.9681720567298,21.));
#8611=CARTESIAN_POINT('Ctrl Pts',(13.4243062623592,-16.9170380509036,0.));
#8612=CARTESIAN_POINT('Ctrl Pts',(13.4243062623592,-16.9170380509036,21.));
#8613=CARTESIAN_POINT('Ctrl Pts',(13.4161718177499,-16.8660160353187,0.));
#8614=CARTESIAN_POINT('Ctrl Pts',(13.4161718177499,-16.8660160353187,21.));
#8615=CARTESIAN_POINT('Ctrl Pts',(13.4077997088426,-16.8151077630226,0.));
#8616=CARTESIAN_POINT('Ctrl Pts',(13.4077997088426,-16.8151077630226,21.));
#8617=CARTESIAN_POINT('Ctrl Pts',(13.3991890464165,-16.7643148579873,0.));
#8618=CARTESIAN_POINT('Ctrl Pts',(13.3991890464165,-16.7643148579873,21.));
#8619=CARTESIAN_POINT('Ctrl Pts',(13.3903389370346,-16.7136388432444,0.));
#8620=CARTESIAN_POINT('Ctrl Pts',(13.3903389370346,-16.7136388432444,21.));
#8621=CARTESIAN_POINT('Ctrl Pts',(13.381248462113,-16.6630812012276,0.));
#8622=CARTESIAN_POINT('Ctrl Pts',(13.381248462113,-16.6630812012276,21.));
#8623=CARTESIAN_POINT('Ctrl Pts',(13.3719166600676,-16.612643424234,0.));
#8624=CARTESIAN_POINT('Ctrl Pts',(13.3719166600676,-16.612643424234,21.));
#8625=CARTESIAN_POINT('Ctrl Pts',(13.3623425108873,-16.5623270636327,0.));
#8626=CARTESIAN_POINT('Ctrl Pts',(13.3623425108873,-16.5623270636327,21.));
#8627=CARTESIAN_POINT('Ctrl Pts',(13.3525249163084,-16.5121337902953,0.));
#8628=CARTESIAN_POINT('Ctrl Pts',(13.3525249163084,-16.5121337902953,21.));
#8629=CARTESIAN_POINT('Ctrl Pts',(13.3424627129921,-16.4620653818862,0.));
#8630=CARTESIAN_POINT('Ctrl Pts',(13.3424627129921,-16.4620653818862,21.));
#8631=CARTESIAN_POINT('Ctrl Pts',(13.3321546976812,-16.4121236828756,0.));
#8632=CARTESIAN_POINT('Ctrl Pts',(13.3321546976812,-16.4121236828756,21.));
#8633=CARTESIAN_POINT('Ctrl Pts',(13.3215996524974,-16.3623105703343,0.));
#8634=CARTESIAN_POINT('Ctrl Pts',(13.3215996524974,-16.3623105703343,21.));
#8635=CARTESIAN_POINT('Ctrl Pts',(13.3107963665229,-16.3126279218067,0.));
#8636=CARTESIAN_POINT('Ctrl Pts',(13.3107963665229,-16.3126279218067,21.));
#8637=CARTESIAN_POINT('Ctrl Pts',(13.2997436744733,-16.2630775678735,0.));
#8638=CARTESIAN_POINT('Ctrl Pts',(13.2997436744733,-16.2630775678735,21.));
#8639=CARTESIAN_POINT('Ctrl Pts',(13.2884404210387,-16.2136613184475,0.));
#8640=CARTESIAN_POINT('Ctrl Pts',(13.2884404210387,-16.2136613184475,21.));
#8641=CARTESIAN_POINT('Ctrl Pts',(13.2768853909882,-16.1643810242643,0.));
#8642=CARTESIAN_POINT('Ctrl Pts',(13.2768853909882,-16.1643810242643,21.));
#8643=CARTESIAN_POINT('Ctrl Pts',(13.2650772466062,-16.1152386305152,0.));
#8644=CARTESIAN_POINT('Ctrl Pts',(13.2650772466062,-16.1152386305152,21.));
#8645=CARTESIAN_POINT('Ctrl Pts',(13.2530144750236,-16.0662362238032,0.));
#8646=CARTESIAN_POINT('Ctrl Pts',(13.2530144750236,-16.0662362238032,21.));
#8647=CARTESIAN_POINT('Ctrl Pts',(13.240695304984,-16.0173761036734,0.));
#8648=CARTESIAN_POINT('Ctrl Pts',(13.240695304984,-16.0173761036734,21.));
#8649=CARTESIAN_POINT('Ctrl Pts',(13.2281177675127,-15.9686607385389,0.));
#8650=CARTESIAN_POINT('Ctrl Pts',(13.2281177675127,-15.9686607385389,21.));
#8651=CARTESIAN_POINT('Ctrl Pts',(13.2152798388134,-15.9200926550954,0.));
#8652=CARTESIAN_POINT('Ctrl Pts',(13.2152798388134,-15.9200926550954,21.));
#8653=CARTESIAN_POINT('Ctrl Pts',(13.2021795724682,-15.8716743375555,0.));
#8654=CARTESIAN_POINT('Ctrl Pts',(13.2021795724682,-15.8716743375555,21.));
#8655=CARTESIAN_POINT('Ctrl Pts',(13.1888152101588,-15.8234081427091,0.));
#8656=CARTESIAN_POINT('Ctrl Pts',(13.1888152101588,-15.8234081427091,21.));
#8657=CARTESIAN_POINT('Ctrl Pts',(13.1751853728467,-15.7752961549278,0.));
#8658=CARTESIAN_POINT('Ctrl Pts',(13.1751853728467,-15.7752961549278,21.));
#8659=CARTESIAN_POINT('Ctrl Pts',(13.161288914421,-15.7273402954914,0.));
#8660=CARTESIAN_POINT('Ctrl Pts',(13.161288914421,-15.7273402954914,21.));
#8661=CARTESIAN_POINT('Ctrl Pts',(13.147124558532,-15.6795425955901,0.));
#8662=CARTESIAN_POINT('Ctrl Pts',(13.147124558532,-15.6795425955901,21.));
#8663=CARTESIAN_POINT('Ctrl Pts',(13.1326905726717,-15.6319054413079,0.));
#8664=CARTESIAN_POINT('Ctrl Pts',(13.1326905726717,-15.6319054413079,21.));
#8665=CARTESIAN_POINT('Ctrl Pts',(13.1179844917497,-15.5844317820184,0.));
#8666=CARTESIAN_POINT('Ctrl Pts',(13.1179844917497,-15.5844317820184,21.));
#8667=CARTESIAN_POINT('Ctrl Pts',(13.1030026646917,-15.5371254712111,0.));
#8668=CARTESIAN_POINT('Ctrl Pts',(13.1030026646917,-15.5371254712111,21.));
#8669=CARTESIAN_POINT('Ctrl Pts',(13.087740560189,-15.4899910401523,0.));
#8670=CARTESIAN_POINT('Ctrl Pts',(13.087740560189,-15.4899910401523,21.));
#8671=CARTESIAN_POINT('Ctrl Pts',(13.0721935806302,-15.4430330918328,0.));
#8672=CARTESIAN_POINT('Ctrl Pts',(13.0721935806302,-15.4430330918328,21.));
#8673=CARTESIAN_POINT('Ctrl Pts',(13.0563577967298,-15.3962557545684,0.));
#8674=CARTESIAN_POINT('Ctrl Pts',(13.0563577967298,-15.3962557545684,21.));
#8675=CARTESIAN_POINT('Ctrl Pts',(13.0402305665115,-15.3496622219036,0.));
#8676=CARTESIAN_POINT('Ctrl Pts',(13.0402305665115,-15.3496622219036,21.));
#8677=CARTESIAN_POINT('Ctrl Pts',(13.0238115816728,-15.3032539741328,0.));
#8678=CARTESIAN_POINT('Ctrl Pts',(13.0238115816728,-15.3032539741328,21.));
#8679=CARTESIAN_POINT('Ctrl Pts',(13.0071020851025,-15.2570313635503,0.));
#8680=CARTESIAN_POINT('Ctrl Pts',(13.0071020851025,-15.2570313635503,21.));
#8681=CARTESIAN_POINT('Ctrl Pts',(12.9901029059182,-15.2109950816083,0.));
#8682=CARTESIAN_POINT('Ctrl Pts',(12.9901029059182,-15.2109950816083,21.));
#8683=CARTESIAN_POINT('Ctrl Pts',(12.9728126886697,-15.1651474813659,0.));
#8684=CARTESIAN_POINT('Ctrl Pts',(12.9728126886697,-15.1651474813659,21.));
#8685=CARTESIAN_POINT('Ctrl Pts',(12.9552263908864,-15.1194937003528,0.));
#8686=CARTESIAN_POINT('Ctrl Pts',(12.9552263908864,-15.1194937003528,21.));
#8687=CARTESIAN_POINT('Ctrl Pts',(12.9373327960422,-15.0740435169624,0.));
#8688=CARTESIAN_POINT('Ctrl Pts',(12.9373327960422,-15.0740435169624,21.));
#8689=CARTESIAN_POINT('Ctrl Pts',(12.9191164383568,-15.0288099208306,0.));
#8690=CARTESIAN_POINT('Ctrl Pts',(12.9191164383568,-15.0288099208306,21.));
#8691=CARTESIAN_POINT('Ctrl Pts',(12.9005620742036,-14.9838057866976,0.));
#8692=CARTESIAN_POINT('Ctrl Pts',(12.9005620742036,-14.9838057866976,21.));
#8693=CARTESIAN_POINT('Ctrl Pts',(12.8816587472147,-14.9390408507356,0.));
#8694=CARTESIAN_POINT('Ctrl Pts',(12.8816587472147,-14.9390408507356,21.));
#8695=CARTESIAN_POINT('Ctrl Pts',(12.8624032236317,-14.8945191569251,0.));
#8696=CARTESIAN_POINT('Ctrl Pts',(12.8624032236317,-14.8945191569251,21.));
#8697=CARTESIAN_POINT('Ctrl Pts',(12.8428057266944,-14.8502347891476,0.));
#8698=CARTESIAN_POINT('Ctrl Pts',(12.8428057266944,-14.8502347891476,21.));
#8699=CARTESIAN_POINT('Ctrl Pts',(12.822884601679,-14.8061758577898,0.));
#8700=CARTESIAN_POINT('Ctrl Pts',(12.822884601679,-14.8061758577898,21.));
#8701=CARTESIAN_POINT('Ctrl Pts',(12.8026557145457,-14.7623324139791,0.));
#8702=CARTESIAN_POINT('Ctrl Pts',(12.8026557145457,-14.7623324139791,21.));
#8703=CARTESIAN_POINT('Ctrl Pts',(12.7821227233337,-14.7187037124277,0.));
#8704=CARTESIAN_POINT('Ctrl Pts',(12.7821227233337,-14.7187037124277,21.));
#8705=CARTESIAN_POINT('Ctrl Pts',(12.7612687078867,-14.6753044633399,0.));
#8706=CARTESIAN_POINT('Ctrl Pts',(12.7612687078867,-14.6753044633399,21.));
#8707=CARTESIAN_POINT('Ctrl Pts',(12.7400427996251,-14.6321748083434,0.));
#8708=CARTESIAN_POINT('Ctrl Pts',(12.7400427996251,-14.6321748083434,21.));
#8709=CARTESIAN_POINT('Ctrl Pts',(12.7183743139638,-14.5893698147583,0.));
#8710=CARTESIAN_POINT('Ctrl Pts',(12.7183743139638,-14.5893698147583,21.));
#8711=CARTESIAN_POINT('Ctrl Pts',(12.6961966430455,-14.5469417071952,0.));
#8712=CARTESIAN_POINT('Ctrl Pts',(12.6961966430455,-14.5469417071952,21.));
#8713=CARTESIAN_POINT('Ctrl Pts',(12.6734695081852,-14.5049233087958,0.));
#8714=CARTESIAN_POINT('Ctrl Pts',(12.6734695081852,-14.5049233087958,21.));
#8715=CARTESIAN_POINT('Ctrl Pts',(12.6501984687124,-14.463313553928,0.));
#8716=CARTESIAN_POINT('Ctrl Pts',(12.6501984687124,-14.463313553928,21.));
#8717=CARTESIAN_POINT('Ctrl Pts',(12.626464614311,-14.4220553460485,0.));
#8718=CARTESIAN_POINT('Ctrl Pts',(12.626464614311,-14.4220553460485,21.));
#8719=CARTESIAN_POINT('Ctrl Pts',(12.6023830189244,-14.3810669346235,0.));
#8720=CARTESIAN_POINT('Ctrl Pts',(12.6023830189244,-14.3810669346235,21.));
#8721=CARTESIAN_POINT('Ctrl Pts',(12.5780443898087,-14.3402859058353,0.));
#8722=CARTESIAN_POINT('Ctrl Pts',(12.5780443898087,-14.3402859058353,21.));
#8723=CARTESIAN_POINT('Ctrl Pts',(12.5534605602317,-14.2997103098726,0.));
#8724=CARTESIAN_POINT('Ctrl Pts',(12.5534605602317,-14.2997103098726,21.));
#8725=CARTESIAN_POINT('Ctrl Pts',(12.5285125321527,-14.2594378207584,0.));
#8726=CARTESIAN_POINT('Ctrl Pts',(12.5285125321527,-14.2594378207584,21.));
#8727=CARTESIAN_POINT('Ctrl Pts',(12.502885965175,-14.2197144660135,0.));
#8728=CARTESIAN_POINT('Ctrl Pts',(12.502885965175,-14.2197144660135,21.));
#8729=CARTESIAN_POINT('Ctrl Pts',(12.4761570639125,-14.1808688343892,0.));
#8730=CARTESIAN_POINT('Ctrl Pts',(12.4761570639125,-14.1808688343892,21.));
#8731=CARTESIAN_POINT('Ctrl Pts',(12.4535485619996,-14.1507598477672,0.));
#8732=CARTESIAN_POINT('Ctrl Pts',(12.4535485619996,-14.1507598477672,21.));
#8733=CARTESIAN_POINT('Ctrl Pts',(12.4357509724316,-14.1288394445866,0.));
#8734=CARTESIAN_POINT('Ctrl Pts',(12.4357509724316,-14.1288394445866,21.));
#8735=CARTESIAN_POINT('Ctrl Pts',(12.4234926340671,-14.1145347042316,0.));
#8736=CARTESIAN_POINT('Ctrl Pts',(12.4234926340671,-14.1145347042316,21.));
#8737=CARTESIAN_POINT('Ctrl Pts',(12.4172651441477,-14.1074595503134,0.));
#8738=CARTESIAN_POINT('Ctrl Pts',(12.4172651441477,-14.1074595503134,21.));
#8739=CARTESIAN_POINT('',(13.4869019493419,-17.3811241238545,0.));
#8740=CARTESIAN_POINT('Ctrl Pts',(12.4172651441477,-14.1074595503134,0.));
#8741=CARTESIAN_POINT('Ctrl Pts',(12.4234926340671,-14.1145347042316,0.));
#8742=CARTESIAN_POINT('Ctrl Pts',(12.4357509724316,-14.1288394445866,0.));
#8743=CARTESIAN_POINT('Ctrl Pts',(12.4535485619996,-14.1507598477672,0.));
#8744=CARTESIAN_POINT('Ctrl Pts',(12.4761570639125,-14.1808688343892,0.));
#8745=CARTESIAN_POINT('Ctrl Pts',(12.502885965175,-14.2197144660135,0.));
#8746=CARTESIAN_POINT('Ctrl Pts',(12.5285125321527,-14.2594378207584,0.));
#8747=CARTESIAN_POINT('Ctrl Pts',(12.5534605602317,-14.2997103098726,0.));
#8748=CARTESIAN_POINT('Ctrl Pts',(12.5780443898087,-14.3402859058353,0.));
#8749=CARTESIAN_POINT('Ctrl Pts',(12.6023830189244,-14.3810669346235,0.));
#8750=CARTESIAN_POINT('Ctrl Pts',(12.626464614311,-14.4220553460485,0.));
#8751=CARTESIAN_POINT('Ctrl Pts',(12.6501984687124,-14.463313553928,0.));
#8752=CARTESIAN_POINT('Ctrl Pts',(12.6734695081852,-14.5049233087958,0.));
#8753=CARTESIAN_POINT('Ctrl Pts',(12.6961966430455,-14.5469417071952,0.));
#8754=CARTESIAN_POINT('Ctrl Pts',(12.7183743139638,-14.5893698147583,0.));
#8755=CARTESIAN_POINT('Ctrl Pts',(12.7400427996251,-14.6321748083434,0.));
#8756=CARTESIAN_POINT('Ctrl Pts',(12.7612687078867,-14.6753044633399,0.));
#8757=CARTESIAN_POINT('Ctrl Pts',(12.7821227233337,-14.7187037124277,0.));
#8758=CARTESIAN_POINT('Ctrl Pts',(12.8026557145457,-14.7623324139791,0.));
#8759=CARTESIAN_POINT('Ctrl Pts',(12.822884601679,-14.8061758577898,0.));
#8760=CARTESIAN_POINT('Ctrl Pts',(12.8428057266944,-14.8502347891476,0.));
#8761=CARTESIAN_POINT('Ctrl Pts',(12.8624032236317,-14.8945191569251,0.));
#8762=CARTESIAN_POINT('Ctrl Pts',(12.8816587472147,-14.9390408507356,0.));
#8763=CARTESIAN_POINT('Ctrl Pts',(12.9005620742036,-14.9838057866976,0.));
#8764=CARTESIAN_POINT('Ctrl Pts',(12.9191164383568,-15.0288099208306,0.));
#8765=CARTESIAN_POINT('Ctrl Pts',(12.9373327960422,-15.0740435169624,0.));
#8766=CARTESIAN_POINT('Ctrl Pts',(12.9552263908864,-15.1194937003528,0.));
#8767=CARTESIAN_POINT('Ctrl Pts',(12.9728126886697,-15.1651474813659,0.));
#8768=CARTESIAN_POINT('Ctrl Pts',(12.9901029059182,-15.2109950816083,0.));
#8769=CARTESIAN_POINT('Ctrl Pts',(13.0071020851025,-15.2570313635503,0.));
#8770=CARTESIAN_POINT('Ctrl Pts',(13.0238115816728,-15.3032539741328,0.));
#8771=CARTESIAN_POINT('Ctrl Pts',(13.0402305665115,-15.3496622219036,0.));
#8772=CARTESIAN_POINT('Ctrl Pts',(13.0563577967298,-15.3962557545684,0.));
#8773=CARTESIAN_POINT('Ctrl Pts',(13.0721935806302,-15.4430330918328,0.));
#8774=CARTESIAN_POINT('Ctrl Pts',(13.087740560189,-15.4899910401523,0.));
#8775=CARTESIAN_POINT('Ctrl Pts',(13.1030026646917,-15.5371254712111,0.));
#8776=CARTESIAN_POINT('Ctrl Pts',(13.1179844917497,-15.5844317820184,0.));
#8777=CARTESIAN_POINT('Ctrl Pts',(13.1326905726717,-15.6319054413079,0.));
#8778=CARTESIAN_POINT('Ctrl Pts',(13.147124558532,-15.6795425955901,0.));
#8779=CARTESIAN_POINT('Ctrl Pts',(13.161288914421,-15.7273402954914,0.));
#8780=CARTESIAN_POINT('Ctrl Pts',(13.1751853728467,-15.7752961549278,0.));
#8781=CARTESIAN_POINT('Ctrl Pts',(13.1888152101588,-15.8234081427091,0.));
#8782=CARTESIAN_POINT('Ctrl Pts',(13.2021795724682,-15.8716743375555,0.));
#8783=CARTESIAN_POINT('Ctrl Pts',(13.2152798388134,-15.9200926550954,0.));
#8784=CARTESIAN_POINT('Ctrl Pts',(13.2281177675127,-15.9686607385389,0.));
#8785=CARTESIAN_POINT('Ctrl Pts',(13.240695304984,-16.0173761036734,0.));
#8786=CARTESIAN_POINT('Ctrl Pts',(13.2530144750236,-16.0662362238032,0.));
#8787=CARTESIAN_POINT('Ctrl Pts',(13.2650772466062,-16.1152386305152,0.));
#8788=CARTESIAN_POINT('Ctrl Pts',(13.2768853909882,-16.1643810242643,0.));
#8789=CARTESIAN_POINT('Ctrl Pts',(13.2884404210387,-16.2136613184475,0.));
#8790=CARTESIAN_POINT('Ctrl Pts',(13.2997436744733,-16.2630775678735,0.));
#8791=CARTESIAN_POINT('Ctrl Pts',(13.3107963665229,-16.3126279218067,0.));
#8792=CARTESIAN_POINT('Ctrl Pts',(13.3215996524974,-16.3623105703343,0.));
#8793=CARTESIAN_POINT('Ctrl Pts',(13.3321546976812,-16.4121236828756,0.));
#8794=CARTESIAN_POINT('Ctrl Pts',(13.3424627129921,-16.4620653818862,0.));
#8795=CARTESIAN_POINT('Ctrl Pts',(13.3525249163084,-16.5121337902953,0.));
#8796=CARTESIAN_POINT('Ctrl Pts',(13.3623425108873,-16.5623270636327,0.));
#8797=CARTESIAN_POINT('Ctrl Pts',(13.3719166600676,-16.612643424234,0.));
#8798=CARTESIAN_POINT('Ctrl Pts',(13.381248462113,-16.6630812012276,0.));
#8799=CARTESIAN_POINT('Ctrl Pts',(13.3903389370346,-16.7136388432444,0.));
#8800=CARTESIAN_POINT('Ctrl Pts',(13.3991890464165,-16.7643148579873,0.));
#8801=CARTESIAN_POINT('Ctrl Pts',(13.4077997088426,-16.8151077630226,0.));
#8802=CARTESIAN_POINT('Ctrl Pts',(13.4161718177499,-16.8660160353187,0.));
#8803=CARTESIAN_POINT('Ctrl Pts',(13.4243062623592,-16.9170380509036,0.));
#8804=CARTESIAN_POINT('Ctrl Pts',(13.432203941793,-16.9681720567298,0.));
#8805=CARTESIAN_POINT('Ctrl Pts',(13.4398657451291,-17.0194162803447,0.));
#8806=CARTESIAN_POINT('Ctrl Pts',(13.4472925380889,-17.0707690194412,0.));
#8807=CARTESIAN_POINT('Ctrl Pts',(13.4544851484583,-17.1222287365697,0.));
#8808=CARTESIAN_POINT('Ctrl Pts',(13.4614443545811,-17.173794155624,0.));
#8809=CARTESIAN_POINT('Ctrl Pts',(13.4695161752399,-17.235798381426,0.));
#8810=CARTESIAN_POINT('Ctrl Pts',(13.4759526005425,-17.287598725272,0.));
#8811=CARTESIAN_POINT('Ctrl Pts',(13.4809165957478,-17.3291218739796,0.));
#8812=CARTESIAN_POINT('Ctrl Pts',(13.4845355519784,-17.360310805254,0.));
#8813=CARTESIAN_POINT('Ctrl Pts',(13.4869019493419,-17.3811241238545,0.));
#8814=CARTESIAN_POINT('',(13.4869019493419,-17.3811241238545,13.));
#8815=CARTESIAN_POINT('Ctrl Pts',(13.4869019493419,-17.3811241238545,13.));
#8816=CARTESIAN_POINT('Ctrl Pts',(13.475253226354,-17.2786694026925,13.));
#8817=CARTESIAN_POINT('Ctrl Pts',(13.4622625504827,-17.1768129075703,13.));
#8818=CARTESIAN_POINT('Ctrl Pts',(13.4479123002588,-17.0755735571127,13.));
#8819=CARTESIAN_POINT('Ctrl Pts',(13.4241333152838,-16.9078155768783,13.));
#8820=CARTESIAN_POINT('Ctrl Pts',(13.3966181281356,-16.7417653304334,13.));
#8821=CARTESIAN_POINT('Ctrl Pts',(13.365224404591,-16.5776745262699,13.));
#8822=CARTESIAN_POINT('Ctrl Pts',(13.341093348038,-16.4515447134285,13.));
#8823=CARTESIAN_POINT('Ctrl Pts',(13.3146689195875,-16.3265706105421,13.));
#8824=CARTESIAN_POINT('Ctrl Pts',(13.2858665160046,-16.2028831155018,13.));
#8825=CARTESIAN_POINT('Ctrl Pts',(13.2548614253322,-16.0697365193248,13.));
#8826=CARTESIAN_POINT('Ctrl Pts',(13.2211052767355,-15.9380763844706,13.));
#8827=CARTESIAN_POINT('Ctrl Pts',(13.1844379732149,-15.8081115250302,13.));
#8828=CARTESIAN_POINT('Ctrl Pts',(13.1641379552979,-15.7361594390595,13.));
#8829=CARTESIAN_POINT('Ctrl Pts',(13.1429498667048,-15.6647240120097,13.));
#8830=CARTESIAN_POINT('Ctrl Pts',(13.1208442193763,-15.5938437095349,13.));
#8831=CARTESIAN_POINT('Ctrl Pts',(13.0995423541622,-15.5255406814797,13.));
#8832=CARTESIAN_POINT('Ctrl Pts',(13.0773830005582,-15.4577571787722,13.));
#8833=CARTESIAN_POINT('Ctrl Pts',(13.0543129132306,-15.3905488552535,13.));
#8834=CARTESIAN_POINT('Ctrl Pts',(13.0343732800162,-15.3324602446263,13.));
#8835=CARTESIAN_POINT('Ctrl Pts',(13.0137559287811,-15.2747993584641,13.));
#8836=CARTESIAN_POINT('Ctrl Pts',(12.9924643459599,-15.2175748373743,13.));
#8837=CARTESIAN_POINT('Ctrl Pts',(12.9771843404788,-15.1765073881741,13.));
#8838=CARTESIAN_POINT('Ctrl Pts',(12.9615593601403,-15.1356630007799,13.));
#8839=CARTESIAN_POINT('Ctrl Pts',(12.9455599556129,-15.0950681406725,13.));
#8840=CARTESIAN_POINT('Ctrl Pts',(12.9298210808532,-15.055134315759,13.));
#8841=CARTESIAN_POINT('Ctrl Pts',(12.9137147531419,-15.0154457689548,13.));
#8842=CARTESIAN_POINT('Ctrl Pts',(12.8972012565652,-14.9760367892145,13.));
#8843=CARTESIAN_POINT('Ctrl Pts',(12.882883085059,-14.9418668889644,13.));
#8844=CARTESIAN_POINT('Ctrl Pts',(12.8682568221008,-14.9079086467153,13.));
#8845=CARTESIAN_POINT('Ctrl Pts',(12.8533364079406,-14.8741550424562,13.));
#8846=CARTESIAN_POINT('Ctrl Pts',(12.839821936482,-14.8435820223986,13.));
#8847=CARTESIAN_POINT('Ctrl Pts',(12.8260705989223,-14.8131735651743,13.));
#8848=CARTESIAN_POINT('Ctrl Pts',(12.8121025760339,-14.7829174093268,13.));
#8849=CARTESIAN_POINT('Ctrl Pts',(12.8003366511334,-14.7574312213154,13.));
#8850=CARTESIAN_POINT('Ctrl Pts',(12.7884183714705,-14.7320520624089,13.));
#8851=CARTESIAN_POINT('Ctrl Pts',(12.7763327022737,-14.7067929861541,13.));
#8852=CARTESIAN_POINT('Ctrl Pts',(12.7588434233209,-14.6702403531541,13.));
#8853=CARTESIAN_POINT('Ctrl Pts',(12.7410029355634,-14.6339396293391,13.));
#8854=CARTESIAN_POINT('Ctrl Pts',(12.7226389619075,-14.5980256537221,13.));
#8855=CARTESIAN_POINT('Ctrl Pts',(12.7115427371053,-14.5763250373713,13.));
#8856=CARTESIAN_POINT('Ctrl Pts',(12.7002526008255,-14.5547677198027,13.));
#8857=CARTESIAN_POINT('Ctrl Pts',(12.6887481997665,-14.5333705425118,13.));
#8858=CARTESIAN_POINT('Ctrl Pts',(12.6781379055282,-14.5136363255141,13.));
#8859=CARTESIAN_POINT('Ctrl Pts',(12.6673442953663,-14.4940391161015,13.));
#8860=CARTESIAN_POINT('Ctrl Pts',(12.656388173486,-14.4745649057707,13.));
#8861=CARTESIAN_POINT('Ctrl Pts',(12.6413169180704,-14.4477761568762,13.));
#8862=CARTESIAN_POINT('Ctrl Pts',(12.6259439377051,-14.4212156950105,13.));
#8863=CARTESIAN_POINT('Ctrl Pts',(12.6103925841804,-14.3947967980687,13.));
#8864=CARTESIAN_POINT('Ctrl Pts',(12.6005265277414,-14.3780361779808,13.));
#8865=CARTESIAN_POINT('Ctrl Pts',(12.5905900370726,-14.3613315562137,13.));
#8866=CARTESIAN_POINT('Ctrl Pts',(12.5805908896517,-14.3446791501185,13.));
#8867=CARTESIAN_POINT('Ctrl Pts',(12.5716171202699,-14.3297343907646,13.));
#8868=CARTESIAN_POINT('Ctrl Pts',(12.5625934694456,-14.3148312514246,13.));
#8869=CARTESIAN_POINT('Ctrl Pts',(12.5534931964106,-14.2999916563736,13.));
#8870=CARTESIAN_POINT('Ctrl Pts',(12.5439269970518,-14.2843922865399,13.));
#8871=CARTESIAN_POINT('Ctrl Pts',(12.534276259247,-14.2688630443264,13.));
#8872=CARTESIAN_POINT('Ctrl Pts',(12.524460288528,-14.2534670740992,13.));
#8873=CARTESIAN_POINT('Ctrl Pts',(12.5081559827695,-14.2278944014392,13.));
#8874=CARTESIAN_POINT('Ctrl Pts',(12.4913891919205,-14.2026946289112,13.));
#8875=CARTESIAN_POINT('Ctrl Pts',(12.4736648236276,-14.1782508276066,13.));
#8876=CARTESIAN_POINT('Ctrl Pts',(12.4638909761914,-14.1647716456823,13.));
#8877=CARTESIAN_POINT('Ctrl Pts',(12.453824835945,-14.1515231428882,13.));
#8878=CARTESIAN_POINT('Ctrl Pts',(12.4434054355307,-14.138552318439,13.));
#8879=CARTESIAN_POINT('Ctrl Pts',(12.4349297906175,-14.128001221649,13.));
#8880=CARTESIAN_POINT('Ctrl Pts',(12.4262204477597,-14.1176338183186,13.));
#8881=CARTESIAN_POINT('Ctrl Pts',(12.4172651441477,-14.1074595503134,13.));
#8882=CARTESIAN_POINT('',(13.4869019493419,-17.3811241238545,0.));
#8883=CARTESIAN_POINT('Origin',(3.33073116609659E-12,-4.58435815896522E-12,
0.));
#8884=CARTESIAN_POINT('',(12.3627494547115,-18.1978687191668,0.));
#8885=CARTESIAN_POINT('Origin',(3.33073116609659E-12,-4.58435815896522E-12,
0.));
#8886=CARTESIAN_POINT('',(12.3627494547115,-18.1978687191668,13.));
#8887=CARTESIAN_POINT('Origin',(3.33073116609659E-12,-4.58435815896522E-12,
13.));
#8888=CARTESIAN_POINT('',(12.3627494547115,-18.1978687191668,0.));
#8889=CARTESIAN_POINT('Ctrl Pts',(9.57984538049454,-16.1689656784104,0.));
#8890=CARTESIAN_POINT('Ctrl Pts',(9.57984538049454,-16.1689656784104,21.));
#8891=CARTESIAN_POINT('Ctrl Pts',(9.58464985151482,-16.1770747160769,0.));
#8892=CARTESIAN_POINT('Ctrl Pts',(9.58464985151482,-16.1770747160769,21.));
#8893=CARTESIAN_POINT('Ctrl Pts',(9.59446643316596,-16.1931534965272,0.));
#8894=CARTESIAN_POINT('Ctrl Pts',(9.59446643316596,-16.1931534965272,21.));
#8895=CARTESIAN_POINT('Ctrl Pts',(9.60981421781523,-16.2168537871666,0.));
#8896=CARTESIAN_POINT('Ctrl Pts',(9.60981421781523,-16.2168537871666,21.));
#8897=CARTESIAN_POINT('Ctrl Pts',(9.63146315443272,-16.2476599387841,0.));
#8898=CARTESIAN_POINT('Ctrl Pts',(9.63146315443272,-16.2476599387841,21.));
#8899=CARTESIAN_POINT('Ctrl Pts',(9.66014786078746,-16.2850845948324,0.));
#8900=CARTESIAN_POINT('Ctrl Pts',(9.66014786078746,-16.2850845948324,21.));
#8901=CARTESIAN_POINT('Ctrl Pts',(9.69000797146315,-16.3217321000366,0.));
#8902=CARTESIAN_POINT('Ctrl Pts',(9.69000797146315,-16.3217321000366,21.));
#8903=CARTESIAN_POINT('Ctrl Pts',(9.72060002001011,-16.3579039682519,0.));
#8904=CARTESIAN_POINT('Ctrl Pts',(9.72060002001011,-16.3579039682519,21.));
#8905=CARTESIAN_POINT('Ctrl Pts',(9.75159288382684,-16.3938231282759,0.));
#8906=CARTESIAN_POINT('Ctrl Pts',(9.75159288382684,-16.3938231282759,21.));
#8907=CARTESIAN_POINT('Ctrl Pts',(9.78285689698057,-16.4295725710378,0.));
#8908=CARTESIAN_POINT('Ctrl Pts',(9.78285689698057,-16.4295725710378,21.));
#8909=CARTESIAN_POINT('Ctrl Pts',(9.81439757053278,-16.4651416449558,0.));
#8910=CARTESIAN_POINT('Ctrl Pts',(9.81439757053278,-16.4651416449558,21.));
#8911=CARTESIAN_POINT('Ctrl Pts',(9.84630229363521,-16.5004633692332,0.));
#8912=CARTESIAN_POINT('Ctrl Pts',(9.84630229363521,-16.5004633692332,21.));
#8913=CARTESIAN_POINT('Ctrl Pts',(9.87868437546979,-16.5354535643506,0.));
#8914=CARTESIAN_POINT('Ctrl Pts',(9.87868437546979,-16.5354535643506,21.));
#8915=CARTESIAN_POINT('Ctrl Pts',(9.91162317616648,-16.5700527532381,0.));
#8916=CARTESIAN_POINT('Ctrl Pts',(9.91162317616648,-16.5700527532381,21.));
#8917=CARTESIAN_POINT('Ctrl Pts',(9.9451214271291,-16.6042559779574,0.));
#8918=CARTESIAN_POINT('Ctrl Pts',(9.9451214271291,-16.6042559779574,21.));
#8919=CARTESIAN_POINT('Ctrl Pts',(9.97913546489641,-16.6380914029057,0.));
#8920=CARTESIAN_POINT('Ctrl Pts',(9.97913546489641,-16.6380914029057,21.));
#8921=CARTESIAN_POINT('Ctrl Pts',(10.0135950379525,-16.6716062376277,0.));
#8922=CARTESIAN_POINT('Ctrl Pts',(10.0135950379525,-16.6716062376277,21.));
#8923=CARTESIAN_POINT('Ctrl Pts',(10.0484259314257,-16.7048506904207,0.));
#8924=CARTESIAN_POINT('Ctrl Pts',(10.0484259314257,-16.7048506904207,21.));
#8925=CARTESIAN_POINT('Ctrl Pts',(10.0835742491038,-16.7378607357337,0.));
#8926=CARTESIAN_POINT('Ctrl Pts',(10.0835742491038,-16.7378607357337,21.));
#8927=CARTESIAN_POINT('Ctrl Pts',(10.1190207721353,-16.7706479198888,0.));
#8928=CARTESIAN_POINT('Ctrl Pts',(10.1190207721353,-16.7706479198888,21.));
#8929=CARTESIAN_POINT('Ctrl Pts',(10.1547673397274,-16.8032089941901,0.));
#8930=CARTESIAN_POINT('Ctrl Pts',(10.1547673397274,-16.8032089941901,21.));
#8931=CARTESIAN_POINT('Ctrl Pts',(10.1908283166713,-16.8355319435838,0.));
#8932=CARTESIAN_POINT('Ctrl Pts',(10.1908283166713,-16.8355319435838,21.));
#8933=CARTESIAN_POINT('Ctrl Pts',(10.2272206796636,-16.8676029947679,0.));
#8934=CARTESIAN_POINT('Ctrl Pts',(10.2272206796636,-16.8676029947679,21.));
#8935=CARTESIAN_POINT('Ctrl Pts',(10.2639532144219,-16.8994142530447,0.));
#8936=CARTESIAN_POINT('Ctrl Pts',(10.2639532144219,-16.8994142530447,21.));
#8937=CARTESIAN_POINT('Ctrl Pts',(10.3010210756062,-16.9309675442426,0.));
#8938=CARTESIAN_POINT('Ctrl Pts',(10.3010210756062,-16.9309675442426,21.));
#8939=CARTESIAN_POINT('Ctrl Pts',(10.3384116178624,-16.9622702798438,0.));
#8940=CARTESIAN_POINT('Ctrl Pts',(10.3384116178624,-16.9622702798438,21.));
#8941=CARTESIAN_POINT('Ctrl Pts',(10.3761078860454,-16.9933329788855,0.));
#8942=CARTESIAN_POINT('Ctrl Pts',(10.3761078860454,-16.9933329788855,21.));
#8943=CARTESIAN_POINT('Ctrl Pts',(10.4140927470882,-17.0241663361802,0.));
#8944=CARTESIAN_POINT('Ctrl Pts',(10.4140927470882,-17.0241663361802,21.));
#8945=CARTESIAN_POINT('Ctrl Pts',(10.452353435089,-17.0547779975888,0.));
#8946=CARTESIAN_POINT('Ctrl Pts',(10.452353435089,-17.0547779975888,21.));
#8947=CARTESIAN_POINT('Ctrl Pts',(10.4908835057575,-17.0851711712016,0.));
#8948=CARTESIAN_POINT('Ctrl Pts',(10.4908835057575,-17.0851711712016,21.));
#8949=CARTESIAN_POINT('Ctrl Pts',(10.5296803023445,-17.1153464189932,0.));
#8950=CARTESIAN_POINT('Ctrl Pts',(10.5296803023445,-17.1153464189932,21.));
#8951=CARTESIAN_POINT('Ctrl Pts',(10.5687434234512,-17.1453027387554,0.));
#8952=CARTESIAN_POINT('Ctrl Pts',(10.5687434234512,-17.1453027387554,21.));
#8953=CARTESIAN_POINT('Ctrl Pts',(10.6080729180997,-17.1750388395657,0.));
#8954=CARTESIAN_POINT('Ctrl Pts',(10.6080729180997,-17.1750388395657,21.));
#8955=CARTESIAN_POINT('Ctrl Pts',(10.6476672831754,-17.2045545572011,0.));
#8956=CARTESIAN_POINT('Ctrl Pts',(10.6476672831754,-17.2045545572011,21.));
#8957=CARTESIAN_POINT('Ctrl Pts',(10.6875226650217,-17.2338514174708,0.));
#8958=CARTESIAN_POINT('Ctrl Pts',(10.6875226650217,-17.2338514174708,21.));
#8959=CARTESIAN_POINT('Ctrl Pts',(10.7276339231608,-17.2629318816279,0.));
#8960=CARTESIAN_POINT('Ctrl Pts',(10.7276339231608,-17.2629318816279,21.));
#8961=CARTESIAN_POINT('Ctrl Pts',(10.7679952591482,-17.2917988998581,0.));
#8962=CARTESIAN_POINT('Ctrl Pts',(10.7679952591482,-17.2917988998581,21.));
#8963=CARTESIAN_POINT('Ctrl Pts',(10.8086009632423,-17.3204553814537,0.));
#8964=CARTESIAN_POINT('Ctrl Pts',(10.8086009632423,-17.3204553814537,21.));
#8965=CARTESIAN_POINT('Ctrl Pts',(10.8494462423127,-17.3489036079991,0.));
#8966=CARTESIAN_POINT('Ctrl Pts',(10.8494462423127,-17.3489036079991,21.));
#8967=CARTESIAN_POINT('Ctrl Pts',(10.8905275295837,-17.377145012528,0.));
#8968=CARTESIAN_POINT('Ctrl Pts',(10.8905275295837,-17.377145012528,21.));
#8969=CARTESIAN_POINT('Ctrl Pts',(10.9318420203801,-17.4051805054129,0.));
#8970=CARTESIAN_POINT('Ctrl Pts',(10.9318420203801,-17.4051805054129,21.));
#8971=CARTESIAN_POINT('Ctrl Pts',(10.9733873885115,-17.4330106728622,0.));
#8972=CARTESIAN_POINT('Ctrl Pts',(10.9733873885115,-17.4330106728622,21.));
#8973=CARTESIAN_POINT('Ctrl Pts',(11.0151614525642,-17.460636011184,0.));
#8974=CARTESIAN_POINT('Ctrl Pts',(11.0151614525642,-17.460636011184,21.));
#8975=CARTESIAN_POINT('Ctrl Pts',(11.0571618040371,-17.4880571878157,0.));
#8976=CARTESIAN_POINT('Ctrl Pts',(11.0571618040371,-17.4880571878157,21.));
#8977=CARTESIAN_POINT('Ctrl Pts',(11.0993856581394,-17.5152751467292,0.));
#8978=CARTESIAN_POINT('Ctrl Pts',(11.0993856581394,-17.5152751467292,21.));
#8979=CARTESIAN_POINT('Ctrl Pts',(11.1418300507683,-17.5422909714139,0.));
#8980=CARTESIAN_POINT('Ctrl Pts',(11.1418300507683,-17.5422909714139,21.));
#8981=CARTESIAN_POINT('Ctrl Pts',(11.1844919535058,-17.5691058058227,0.));
#8982=CARTESIAN_POINT('Ctrl Pts',(11.1844919535058,-17.5691058058227,21.));
#8983=CARTESIAN_POINT('Ctrl Pts',(11.2273684103051,-17.5957207597803,0.));
#8984=CARTESIAN_POINT('Ctrl Pts',(11.2273684103051,-17.5957207597803,21.));
#8985=CARTESIAN_POINT('Ctrl Pts',(11.2704566868205,-17.6221368072528,0.));
#8986=CARTESIAN_POINT('Ctrl Pts',(11.2704566868205,-17.6221368072528,21.));
#8987=CARTESIAN_POINT('Ctrl Pts',(11.3137543310722,-17.6483547422688,0.));
#8988=CARTESIAN_POINT('Ctrl Pts',(11.3137543310722,-17.6483547422688,21.));
#8989=CARTESIAN_POINT('Ctrl Pts',(11.3572590796967,-17.674375235974,0.));
#8990=CARTESIAN_POINT('Ctrl Pts',(11.3572590796967,-17.674375235974,21.));
#8991=CARTESIAN_POINT('Ctrl Pts',(11.4009687970126,-17.700198872213,0.));
#8992=CARTESIAN_POINT('Ctrl Pts',(11.4009687970126,-17.700198872213,21.));
#8993=CARTESIAN_POINT('Ctrl Pts',(11.4448814046804,-17.725826190457,0.));
#8994=CARTESIAN_POINT('Ctrl Pts',(11.4448814046804,-17.725826190457,21.));
#8995=CARTESIAN_POINT('Ctrl Pts',(11.4889948016216,-17.7512577332768,0.));
#8996=CARTESIAN_POINT('Ctrl Pts',(11.4889948016216,-17.7512577332768,21.));
#8997=CARTESIAN_POINT('Ctrl Pts',(11.5333068279911,-17.7764940721306,0.));
#8998=CARTESIAN_POINT('Ctrl Pts',(11.5333068279911,-17.7764940721306,21.));
#8999=CARTESIAN_POINT('Ctrl Pts',(11.5778153222435,-17.8015357852426,0.));
#9000=CARTESIAN_POINT('Ctrl Pts',(11.5778153222435,-17.8015357852426,21.));
#9001=CARTESIAN_POINT('Ctrl Pts',(11.6225181583564,-17.8263834470057,0.));
#9002=CARTESIAN_POINT('Ctrl Pts',(11.6225181583564,-17.8263834470057,21.));
#9003=CARTESIAN_POINT('Ctrl Pts',(11.6674132861792,-17.8510376144926,0.));
#9004=CARTESIAN_POINT('Ctrl Pts',(11.6674132861792,-17.8510376144926,21.));
#9005=CARTESIAN_POINT('Ctrl Pts',(11.7124987772363,-17.8754988158862,0.));
#9006=CARTESIAN_POINT('Ctrl Pts',(11.7124987772363,-17.8754988158862,21.));
#9007=CARTESIAN_POINT('Ctrl Pts',(11.7577728408871,-17.8997675418752,0.));
#9008=CARTESIAN_POINT('Ctrl Pts',(11.7577728408871,-17.8997675418752,21.));
#9009=CARTESIAN_POINT('Ctrl Pts',(11.8032337607271,-17.9238442458356,0.));
#9010=CARTESIAN_POINT('Ctrl Pts',(11.8032337607271,-17.9238442458356,21.));
#9011=CARTESIAN_POINT('Ctrl Pts',(11.8488798430201,-17.9477293432951,0.));
#9012=CARTESIAN_POINT('Ctrl Pts',(11.8488798430201,-17.9477293432951,21.));
#9013=CARTESIAN_POINT('Ctrl Pts',(11.8947093631895,-17.9714232133203,0.));
#9014=CARTESIAN_POINT('Ctrl Pts',(11.8947093631895,-17.9714232133203,21.));
#9015=CARTESIAN_POINT('Ctrl Pts',(11.9407205019619,-17.9949261997754,0.));
#9016=CARTESIAN_POINT('Ctrl Pts',(11.9407205019619,-17.9949261997754,21.));
#9017=CARTESIAN_POINT('Ctrl Pts',(11.986911314246,-18.0182386160553,0.));
#9018=CARTESIAN_POINT('Ctrl Pts',(11.986911314246,-18.0182386160553,21.));
#9019=CARTESIAN_POINT('Ctrl Pts',(12.0332798395991,-18.0413607600052,0.));
#9020=CARTESIAN_POINT('Ctrl Pts',(12.0332798395991,-18.0413607600052,21.));
#9021=CARTESIAN_POINT('Ctrl Pts',(12.0798241915081,-18.0642929289333,0.));
#9022=CARTESIAN_POINT('Ctrl Pts',(12.0798241915081,-18.0642929289333,21.));
#9023=CARTESIAN_POINT('Ctrl Pts',(12.1265426519718,-18.0870354350128,0.));
#9024=CARTESIAN_POINT('Ctrl Pts',(12.1265426519718,-18.0870354350128,21.));
#9025=CARTESIAN_POINT('Ctrl Pts',(12.1734337668195,-18.109588624154,0.));
#9026=CARTESIAN_POINT('Ctrl Pts',(12.1734337668195,-18.109588624154,21.));
#9027=CARTESIAN_POINT('Ctrl Pts',(12.2204964278426,-18.1319528884305,0.));
#9028=CARTESIAN_POINT('Ctrl Pts',(12.2204964278426,-18.1319528884305,21.));
#9029=CARTESIAN_POINT('Ctrl Pts',(12.2677298318549,-18.1541286139166,0.));
#9030=CARTESIAN_POINT('Ctrl Pts',(12.2677298318549,-18.1541286139166,21.));
#9031=CARTESIAN_POINT('Ctrl Pts',(12.3056527265146,-18.1717186310224,0.));
#9032=CARTESIAN_POINT('Ctrl Pts',(12.3056527265146,-18.1717186310224,21.));
#9033=CARTESIAN_POINT('Ctrl Pts',(12.3341713636489,-18.1848265584754,0.));
#9034=CARTESIAN_POINT('Ctrl Pts',(12.3341713636489,-18.1848265584754,21.));
#9035=CARTESIAN_POINT('Ctrl Pts',(12.3532177620787,-18.1935275957711,0.));
#9036=CARTESIAN_POINT('Ctrl Pts',(12.3532177620787,-18.1935275957711,21.));
#9037=CARTESIAN_POINT('Ctrl Pts',(12.3627494547115,-18.1978687191668,0.));
#9038=CARTESIAN_POINT('Ctrl Pts',(12.3627494547115,-18.1978687191668,21.));
#9039=CARTESIAN_POINT('Ctrl Pts',(9.57984538049454,-16.1689656784104,0.));
#9040=CARTESIAN_POINT('Ctrl Pts',(9.58464985151482,-16.1770747160769,0.));
#9041=CARTESIAN_POINT('Ctrl Pts',(9.59446643316596,-16.1931534965272,0.));
#9042=CARTESIAN_POINT('Ctrl Pts',(9.60981421781523,-16.2168537871666,0.));
#9043=CARTESIAN_POINT('Ctrl Pts',(9.63146315443272,-16.2476599387841,0.));
#9044=CARTESIAN_POINT('Ctrl Pts',(9.66014786078746,-16.2850845948324,0.));
#9045=CARTESIAN_POINT('Ctrl Pts',(9.69000797146315,-16.3217321000366,0.));
#9046=CARTESIAN_POINT('Ctrl Pts',(9.72060002001011,-16.3579039682519,0.));
#9047=CARTESIAN_POINT('Ctrl Pts',(9.75159288382684,-16.3938231282759,0.));
#9048=CARTESIAN_POINT('Ctrl Pts',(9.78285689698057,-16.4295725710378,0.));
#9049=CARTESIAN_POINT('Ctrl Pts',(9.81439757053278,-16.4651416449558,0.));
#9050=CARTESIAN_POINT('Ctrl Pts',(9.84630229363521,-16.5004633692332,0.));
#9051=CARTESIAN_POINT('Ctrl Pts',(9.87868437546979,-16.5354535643506,0.));
#9052=CARTESIAN_POINT('Ctrl Pts',(9.91162317616648,-16.5700527532381,0.));
#9053=CARTESIAN_POINT('Ctrl Pts',(9.9451214271291,-16.6042559779574,0.));
#9054=CARTESIAN_POINT('Ctrl Pts',(9.97913546489641,-16.6380914029057,0.));
#9055=CARTESIAN_POINT('Ctrl Pts',(10.0135950379525,-16.6716062376277,0.));
#9056=CARTESIAN_POINT('Ctrl Pts',(10.0484259314257,-16.7048506904207,0.));
#9057=CARTESIAN_POINT('Ctrl Pts',(10.0835742491038,-16.7378607357337,0.));
#9058=CARTESIAN_POINT('Ctrl Pts',(10.1190207721353,-16.7706479198888,0.));
#9059=CARTESIAN_POINT('Ctrl Pts',(10.1547673397274,-16.8032089941901,0.));
#9060=CARTESIAN_POINT('Ctrl Pts',(10.1908283166713,-16.8355319435838,0.));
#9061=CARTESIAN_POINT('Ctrl Pts',(10.2272206796636,-16.8676029947679,0.));
#9062=CARTESIAN_POINT('Ctrl Pts',(10.2639532144219,-16.8994142530447,0.));
#9063=CARTESIAN_POINT('Ctrl Pts',(10.3010210756062,-16.9309675442426,0.));
#9064=CARTESIAN_POINT('Ctrl Pts',(10.3384116178624,-16.9622702798438,0.));
#9065=CARTESIAN_POINT('Ctrl Pts',(10.3761078860454,-16.9933329788855,0.));
#9066=CARTESIAN_POINT('Ctrl Pts',(10.4140927470882,-17.0241663361802,0.));
#9067=CARTESIAN_POINT('Ctrl Pts',(10.452353435089,-17.0547779975888,0.));
#9068=CARTESIAN_POINT('Ctrl Pts',(10.4908835057575,-17.0851711712016,0.));
#9069=CARTESIAN_POINT('Ctrl Pts',(10.5296803023445,-17.1153464189932,0.));
#9070=CARTESIAN_POINT('Ctrl Pts',(10.5687434234512,-17.1453027387554,0.));
#9071=CARTESIAN_POINT('Ctrl Pts',(10.6080729180997,-17.1750388395657,0.));
#9072=CARTESIAN_POINT('Ctrl Pts',(10.6476672831754,-17.2045545572011,0.));
#9073=CARTESIAN_POINT('Ctrl Pts',(10.6875226650217,-17.2338514174708,0.));
#9074=CARTESIAN_POINT('Ctrl Pts',(10.7276339231608,-17.2629318816279,0.));
#9075=CARTESIAN_POINT('Ctrl Pts',(10.7679952591482,-17.2917988998581,0.));
#9076=CARTESIAN_POINT('Ctrl Pts',(10.8086009632423,-17.3204553814537,0.));
#9077=CARTESIAN_POINT('Ctrl Pts',(10.8494462423127,-17.3489036079991,0.));
#9078=CARTESIAN_POINT('Ctrl Pts',(10.8905275295837,-17.377145012528,0.));
#9079=CARTESIAN_POINT('Ctrl Pts',(10.9318420203801,-17.4051805054129,0.));
#9080=CARTESIAN_POINT('Ctrl Pts',(10.9733873885115,-17.4330106728622,0.));
#9081=CARTESIAN_POINT('Ctrl Pts',(11.0151614525642,-17.460636011184,0.));
#9082=CARTESIAN_POINT('Ctrl Pts',(11.0571618040371,-17.4880571878157,0.));
#9083=CARTESIAN_POINT('Ctrl Pts',(11.0993856581394,-17.5152751467292,0.));
#9084=CARTESIAN_POINT('Ctrl Pts',(11.1418300507683,-17.5422909714139,0.));
#9085=CARTESIAN_POINT('Ctrl Pts',(11.1844919535058,-17.5691058058227,0.));
#9086=CARTESIAN_POINT('Ctrl Pts',(11.2273684103051,-17.5957207597803,0.));
#9087=CARTESIAN_POINT('Ctrl Pts',(11.2704566868205,-17.6221368072528,0.));
#9088=CARTESIAN_POINT('Ctrl Pts',(11.3137543310722,-17.6483547422688,0.));
#9089=CARTESIAN_POINT('Ctrl Pts',(11.3572590796967,-17.674375235974,0.));
#9090=CARTESIAN_POINT('Ctrl Pts',(11.4009687970126,-17.700198872213,0.));
#9091=CARTESIAN_POINT('Ctrl Pts',(11.4448814046804,-17.725826190457,0.));
#9092=CARTESIAN_POINT('Ctrl Pts',(11.4889948016216,-17.7512577332768,0.));
#9093=CARTESIAN_POINT('Ctrl Pts',(11.5333068279911,-17.7764940721306,0.));
#9094=CARTESIAN_POINT('Ctrl Pts',(11.5778153222435,-17.8015357852426,0.));
#9095=CARTESIAN_POINT('Ctrl Pts',(11.6225181583564,-17.8263834470057,0.));
#9096=CARTESIAN_POINT('Ctrl Pts',(11.6674132861792,-17.8510376144926,0.));
#9097=CARTESIAN_POINT('Ctrl Pts',(11.7124987772363,-17.8754988158862,0.));
#9098=CARTESIAN_POINT('Ctrl Pts',(11.7577728408871,-17.8997675418752,0.));
#9099=CARTESIAN_POINT('Ctrl Pts',(11.8032337607271,-17.9238442458356,0.));
#9100=CARTESIAN_POINT('Ctrl Pts',(11.8488798430201,-17.9477293432951,0.));
#9101=CARTESIAN_POINT('Ctrl Pts',(11.8947093631895,-17.9714232133203,0.));
#9102=CARTESIAN_POINT('Ctrl Pts',(11.9407205019619,-17.9949261997754,0.));
#9103=CARTESIAN_POINT('Ctrl Pts',(11.986911314246,-18.0182386160553,0.));
#9104=CARTESIAN_POINT('Ctrl Pts',(12.0332798395991,-18.0413607600052,0.));
#9105=CARTESIAN_POINT('Ctrl Pts',(12.0798241915081,-18.0642929289333,0.));
#9106=CARTESIAN_POINT('Ctrl Pts',(12.1265426519718,-18.0870354350128,0.));
#9107=CARTESIAN_POINT('Ctrl Pts',(12.1734337668195,-18.109588624154,0.));
#9108=CARTESIAN_POINT('Ctrl Pts',(12.2299089600472,-18.1364257412858,0.));
#9109=CARTESIAN_POINT('Ctrl Pts',(12.2771850498068,-18.1585543320743,0.));
#9110=CARTESIAN_POINT('Ctrl Pts',(12.3151419520839,-18.1761067306718,0.));
#9111=CARTESIAN_POINT('Ctrl Pts',(12.3436860694314,-18.1891864723772,0.));
#9112=CARTESIAN_POINT('Ctrl Pts',(12.3627494547115,-18.1978687191668,0.));
#9113=CARTESIAN_POINT('Ctrl Pts',(9.57984538049454,-16.1689656784104,13.));
#9114=CARTESIAN_POINT('Ctrl Pts',(9.58794311444024,-16.1826331205288,13.));
#9115=CARTESIAN_POINT('Ctrl Pts',(9.59639855902139,-16.196060540494,13.));
#9116=CARTESIAN_POINT('Ctrl Pts',(9.60518801710191,-16.2092641655575,13.));
#9117=CARTESIAN_POINT('Ctrl Pts',(9.61548991937318,-16.2247398016872,13.));
#9118=CARTESIAN_POINT('Ctrl Pts',(9.62624998105864,-16.2399084848403,13.));
#9119=CARTESIAN_POINT('Ctrl Pts',(9.63737105567212,-16.2548366371546,13.));
#9120=CARTESIAN_POINT('Ctrl Pts',(9.65301893987961,-16.2758412618842,13.));
#9121=CARTESIAN_POINT('Ctrl Pts',(9.66937567449445,-16.296373798593,13.));
#9122=CARTESIAN_POINT('Ctrl Pts',(9.6861023820138,-16.3166650331525,13.));
#9123=CARTESIAN_POINT('Ctrl Pts',(9.69722828051143,-16.3301619042994,13.));
#9124=CARTESIAN_POINT('Ctrl Pts',(9.70851618070908,-16.343553146753,13.));
#9125=CARTESIAN_POINT('Ctrl Pts',(9.71989107792203,-16.3568892752803,13.));
#9126=CARTESIAN_POINT('Ctrl Pts',(9.73186502185141,-16.3709277366598,13.));
#9127=CARTESIAN_POINT('Ctrl Pts',(9.74393463777169,-16.3849056240606,13.));
#9128=CARTESIAN_POINT('Ctrl Pts',(9.75606525514033,-16.3988451548263,13.));
#9129=CARTESIAN_POINT('Ctrl Pts',(9.76953696976191,-16.4143257667958,13.));
#9130=CARTESIAN_POINT('Ctrl Pts',(9.78308498747857,-16.4297583183374,13.));
#9131=CARTESIAN_POINT('Ctrl Pts',(9.79671869020116,-16.445133876345,13.));
#9132=CARTESIAN_POINT('Ctrl Pts',(9.81727215878356,-16.4683132763127,13.));
#9133=CARTESIAN_POINT('Ctrl Pts',(9.83802550134714,-16.4913594464763,13.));
#9134=CARTESIAN_POINT('Ctrl Pts',(9.85910360865385,-16.5141788054386,13.));
#9135=CARTESIAN_POINT('Ctrl Pts',(9.87441639279619,-16.530756570841,13.));
#9136=CARTESIAN_POINT('Ctrl Pts',(9.88990330206655,-16.5472127771021,13.));
#9137=CARTESIAN_POINT('Ctrl Pts',(9.90558047214739,-16.5635345032248,13.));
#9138=CARTESIAN_POINT('Ctrl Pts',(9.92474447016412,-16.5834864158106,13.));
#9139=CARTESIAN_POINT('Ctrl Pts',(9.94419173110064,-16.6032381063723,13.));
#9140=CARTESIAN_POINT('Ctrl Pts',(9.96388214930523,-16.6228156007794,13.));
#9141=CARTESIAN_POINT('Ctrl Pts',(9.98515106890727,-16.6439625439386,13.));
#9142=CARTESIAN_POINT('Ctrl Pts',(10.0066988150519,-16.664909699818,13.));
#9143=CARTESIAN_POINT('Ctrl Pts',(10.0284493480894,-16.6857083247985,13.));
#9144=CARTESIAN_POINT('Ctrl Pts',(10.0485293380065,-16.7049095176695,13.));
#9145=CARTESIAN_POINT('Ctrl Pts',(10.0687801145839,-16.7239855768671,13.));
#9146=CARTESIAN_POINT('Ctrl Pts',(10.089177591015,-16.7429517500618,13.));
#9147=CARTESIAN_POINT('Ctrl Pts',(10.1168886100199,-16.7687182701321,13.));
#9148=CARTESIAN_POINT('Ctrl Pts',(10.1448719871897,-16.7942808297091,13.));
#9149=CARTESIAN_POINT('Ctrl Pts',(10.1731502199795,-16.819619458001,13.));
#9150=CARTESIAN_POINT('Ctrl Pts',(10.2004381038856,-16.8440706870545,13.));
#9151=CARTESIAN_POINT('Ctrl Pts',(10.228006930926,-16.868308889081,13.));
#9152=CARTESIAN_POINT('Ctrl Pts',(10.2558682820648,-16.8923226175308,13.));
#9153=CARTESIAN_POINT('Ctrl Pts',(10.2937187080095,-16.9249459402769,13.));
#9154=CARTESIAN_POINT('Ctrl Pts',(10.3321063567311,-16.9571568355792,13.));
#9155=CARTESIAN_POINT('Ctrl Pts',(10.3709578723438,-16.9889999234809,13.));
#9156=CARTESIAN_POINT('Ctrl Pts',(10.4051075099835,-17.0169893055171,13.));
#9157=CARTESIAN_POINT('Ctrl Pts',(10.4396099588442,-17.0446984862637,13.));
#9158=CARTESIAN_POINT('Ctrl Pts',(10.4744368761282,-17.0721430001052,13.));
#9159=CARTESIAN_POINT('Ctrl Pts',(10.5257802080853,-17.1126028769606,13.));
#9160=CARTESIAN_POINT('Ctrl Pts',(10.577836103537,-17.1524822679612,13.));
#9161=CARTESIAN_POINT('Ctrl Pts',(10.630594631353,-17.1917748564007,13.));
#9162=CARTESIAN_POINT('Ctrl Pts',(10.6971764079367,-17.2413624861769,13.));
#9163=CARTESIAN_POINT('Ctrl Pts',(10.764872979571,-17.2900185096906,13.));
#9164=CARTESIAN_POINT('Ctrl Pts',(10.8335716331614,-17.3377983049103,13.));
#9165=CARTESIAN_POINT('Ctrl Pts',(10.9266292560921,-17.402519721341,13.));
#9166=CARTESIAN_POINT('Ctrl Pts',(11.0215303650587,-17.4656299469596,13.));
#9167=CARTESIAN_POINT('Ctrl Pts',(11.1181400566921,-17.5271690591565,13.));
#9168=CARTESIAN_POINT('Ctrl Pts',(11.2042701269916,-17.5820327893897,13.));
#9169=CARTESIAN_POINT('Ctrl Pts',(11.291751266876,-17.6356526672064,13.));
#9170=CARTESIAN_POINT('Ctrl Pts',(11.3804891404118,-17.6880597480309,13.));
#9171=CARTESIAN_POINT('Ctrl Pts',(11.5062551088123,-17.76233499273,13.));
#9172=CARTESIAN_POINT('Ctrl Pts',(11.6345494491014,-17.8341701544337,13.));
#9173=CARTESIAN_POINT('Ctrl Pts',(11.765154236571,-17.9036238130503,13.));
#9174=CARTESIAN_POINT('Ctrl Pts',(11.8666049274963,-17.9575737622862,13.));
#9175=CARTESIAN_POINT('Ctrl Pts',(11.9694546928344,-18.0100864753188,13.));
#9176=CARTESIAN_POINT('Ctrl Pts',(12.073610189358,-18.0611784506835,13.));
#9177=CARTESIAN_POINT('Ctrl Pts',(12.1637125549315,-18.1053768655136,13.));
#9178=CARTESIAN_POINT('Ctrl Pts',(12.2547877907941,-18.1485120961321,13.));
#9179=CARTESIAN_POINT('Ctrl Pts',(12.3468112467815,-18.1905949543846,13.));
#9180=CARTESIAN_POINT('Ctrl Pts',(12.3521208125291,-18.1930230494864,13.));
#9181=CARTESIAN_POINT('Ctrl Pts',(12.357433548566,-18.1954476376835,13.));
#9182=CARTESIAN_POINT('Ctrl Pts',(12.3627494547115,-18.1978687191668,13.));
#9183=CARTESIAN_POINT('Ctrl Pts',(7.455743247944,-20.698113262342,0.));
#9184=CARTESIAN_POINT('Ctrl Pts',(7.455743247944,-20.698113262342,21.));
#9185=CARTESIAN_POINT('Ctrl Pts',(7.45783379370107,-20.6878503127065,0.));
#9186=CARTESIAN_POINT('Ctrl Pts',(7.45783379370107,-20.6878503127065,21.));
#9187=CARTESIAN_POINT('Ctrl Pts',(7.46198969876653,-20.6673271112931,0.));
#9188=CARTESIAN_POINT('Ctrl Pts',(7.46198969876653,-20.6673271112931,21.));
#9189=CARTESIAN_POINT('Ctrl Pts',(7.46814799701905,-20.6365504027501,0.));
#9190=CARTESIAN_POINT('Ctrl Pts',(7.46814799701905,-20.6365504027501,21.));
#9191=CARTESIAN_POINT('Ctrl Pts',(7.47620789245427,-20.5955309838521,0.));
#9192=CARTESIAN_POINT('Ctrl Pts',(7.47620789245427,-20.5955309838521,21.));
#9193=CARTESIAN_POINT('Ctrl Pts',(7.48603045196744,-20.5442837929044,0.));
#9194=CARTESIAN_POINT('Ctrl Pts',(7.48603045196744,-20.5442837929044,21.));
#9195=CARTESIAN_POINT('Ctrl Pts',(7.49560012018405,-20.4930639156161,0.));
#9196=CARTESIAN_POINT('Ctrl Pts',(7.49560012018405,-20.4930639156161,21.));
#9197=CARTESIAN_POINT('Ctrl Pts',(7.50491611266253,-20.4418717748497,0.));
#9198=CARTESIAN_POINT('Ctrl Pts',(7.50491611266253,-20.4418717748497,21.));
#9199=CARTESIAN_POINT('Ctrl Pts',(7.51397746081993,-20.3907080367098,0.));
#9200=CARTESIAN_POINT('Ctrl Pts',(7.51397746081993,-20.3907080367098,21.));
#9201=CARTESIAN_POINT('Ctrl Pts',(7.52278303006887,-20.3395736743243,0.));
#9202=CARTESIAN_POINT('Ctrl Pts',(7.52278303006887,-20.3395736743243,21.));
#9203=CARTESIAN_POINT('Ctrl Pts',(7.53133155804007,-20.2884698940944,0.));
#9204=CARTESIAN_POINT('Ctrl Pts',(7.53133155804007,-20.2884698940944,21.));
#9205=CARTESIAN_POINT('Ctrl Pts',(7.53962169534166,-20.2373980474879,0.));
#9206=CARTESIAN_POINT('Ctrl Pts',(7.53962169534166,-20.2373980474879,21.));
#9207=CARTESIAN_POINT('Ctrl Pts',(7.54765204869254,-20.1863595454674,0.));
#9208=CARTESIAN_POINT('Ctrl Pts',(7.54765204869254,-20.1863595454674,21.));
#9209=CARTESIAN_POINT('Ctrl Pts',(7.55542122125494,-20.1353557774357,0.));
#9210=CARTESIAN_POINT('Ctrl Pts',(7.55542122125494,-20.1353557774357,21.));
#9211=CARTESIAN_POINT('Ctrl Pts',(7.5629278654946,-20.0843880130978,0.));
#9212=CARTESIAN_POINT('Ctrl Pts',(7.5629278654946,-20.0843880130978,21.));
#9213=CARTESIAN_POINT('Ctrl Pts',(7.57017066105972,-20.0334574248557,0.));
#9214=CARTESIAN_POINT('Ctrl Pts',(7.57017066105972,-20.0334574248557,21.));
#9215=CARTESIAN_POINT('Ctrl Pts',(7.57714827622805,-19.9825651387294,0.));
#9216=CARTESIAN_POINT('Ctrl Pts',(7.57714827622805,-19.9825651387294,21.));
#9217=CARTESIAN_POINT('Ctrl Pts',(7.58385933533351,-19.931712276832,0.));
#9218=CARTESIAN_POINT('Ctrl Pts',(7.58385933533351,-19.931712276832,21.));
#9219=CARTESIAN_POINT('Ctrl Pts',(7.59030238888851,-19.8808999994024,0.));
#9220=CARTESIAN_POINT('Ctrl Pts',(7.59030238888851,-19.8808999994024,21.));
#9221=CARTESIAN_POINT('Ctrl Pts',(7.59647587605448,-19.830129556152,0.));
#9222=CARTESIAN_POINT('Ctrl Pts',(7.59647587605448,-19.830129556152,21.));
#9223=CARTESIAN_POINT('Ctrl Pts',(7.60237814110186,-19.7794022782484,0.));
#9224=CARTESIAN_POINT('Ctrl Pts',(7.60237814110186,-19.7794022782484,21.));
#9225=CARTESIAN_POINT('Ctrl Pts',(7.60800746969261,-19.7287195480601,0.));
#9226=CARTESIAN_POINT('Ctrl Pts',(7.60800746969261,-19.7287195480601,21.));
#9227=CARTESIAN_POINT('Ctrl Pts',(7.61336212350878,-19.6780827744426,0.));
#9228=CARTESIAN_POINT('Ctrl Pts',(7.61336212350878,-19.6780827744426,21.));
#9229=CARTESIAN_POINT('Ctrl Pts',(7.6184403707059,-19.6274933688524,0.));
#9230=CARTESIAN_POINT('Ctrl Pts',(7.6184403707059,-19.6274933688524,21.));
#9231=CARTESIAN_POINT('Ctrl Pts',(7.62324053735219,-19.5769527121826,0.));
#9232=CARTESIAN_POINT('Ctrl Pts',(7.62324053735219,-19.5769527121826,21.));
#9233=CARTESIAN_POINT('Ctrl Pts',(7.62776096538882,-19.5264621687521,0.));
#9234=CARTESIAN_POINT('Ctrl Pts',(7.62776096538882,-19.5264621687521,21.));
#9235=CARTESIAN_POINT('Ctrl Pts',(7.63199992715365,-19.4760231231881,0.));
#9236=CARTESIAN_POINT('Ctrl Pts',(7.63199992715365,-19.4760231231881,21.));
#9237=CARTESIAN_POINT('Ctrl Pts',(7.63595554930653,-19.4256370121006,0.));
#9238=CARTESIAN_POINT('Ctrl Pts',(7.63595554930653,-19.4256370121006,21.));
#9239=CARTESIAN_POINT('Ctrl Pts',(7.6396257482276,-19.3753053524647,0.));
#9240=CARTESIAN_POINT('Ctrl Pts',(7.6396257482276,-19.3753053524647,21.));
#9241=CARTESIAN_POINT('Ctrl Pts',(7.64300812875338,-19.3250297839295,0.));
#9242=CARTESIAN_POINT('Ctrl Pts',(7.64300812875338,-19.3250297839295,21.));
#9243=CARTESIAN_POINT('Ctrl Pts',(7.64610005549613,-19.2748120456486,0.));
#9244=CARTESIAN_POINT('Ctrl Pts',(7.64610005549613,-19.2748120456486,21.));
#9245=CARTESIAN_POINT('Ctrl Pts',(7.64889882291923,-19.224653915265,0.));
#9246=CARTESIAN_POINT('Ctrl Pts',(7.64889882291923,-19.224653915265,21.));
#9247=CARTESIAN_POINT('Ctrl Pts',(7.65140181220525,-19.1745571539291,0.));
#9248=CARTESIAN_POINT('Ctrl Pts',(7.65140181220525,-19.1745571539291,21.));
#9249=CARTESIAN_POINT('Ctrl Pts',(7.65360662280608,-19.1245234597312,0.));
#9250=CARTESIAN_POINT('Ctrl Pts',(7.65360662280608,-19.1245234597312,21.));
#9251=CARTESIAN_POINT('Ctrl Pts',(7.65551129907201,-19.0745543888799,0.));
#9252=CARTESIAN_POINT('Ctrl Pts',(7.65551129907201,-19.0745543888799,21.));
#9253=CARTESIAN_POINT('Ctrl Pts',(7.65711415727854,-19.0246514144531,0.));
#9254=CARTESIAN_POINT('Ctrl Pts',(7.65711415727854,-19.0246514144531,21.));
#9255=CARTESIAN_POINT('Ctrl Pts',(7.65841335587266,-18.974816073814,0.));
#9256=CARTESIAN_POINT('Ctrl Pts',(7.65841335587266,-18.974816073814,21.));
#9257=CARTESIAN_POINT('Ctrl Pts',(7.65940650980098,-18.9250501008887,0.));
#9258=CARTESIAN_POINT('Ctrl Pts',(7.65940650980098,-18.9250501008887,21.));
#9259=CARTESIAN_POINT('Ctrl Pts',(7.66009036321662,-18.8753555389435,0.));
#9260=CARTESIAN_POINT('Ctrl Pts',(7.66009036321662,-18.8753555389435,21.));
#9261=CARTESIAN_POINT('Ctrl Pts',(7.66046025294774,-18.8257349246207,0.));
#9262=CARTESIAN_POINT('Ctrl Pts',(7.66046025294774,-18.8257349246207,21.));
#9263=CARTESIAN_POINT('Ctrl Pts',(7.6605104692254,-18.7761911671591,0.));
#9264=CARTESIAN_POINT('Ctrl Pts',(7.6605104692254,-18.7761911671591,21.));
#9265=CARTESIAN_POINT('Ctrl Pts',(7.66023521705904,-18.7267272235231,0.));
#9266=CARTESIAN_POINT('Ctrl Pts',(7.66023521705904,-18.7267272235231,21.));
#9267=CARTESIAN_POINT('Ctrl Pts',(7.65962948375621,-18.6773458057584,0.));
#9268=CARTESIAN_POINT('Ctrl Pts',(7.65962948375621,-18.6773458057584,21.));
#9269=CARTESIAN_POINT('Ctrl Pts',(7.65868976978871,-18.6280491346907,0.));
#9270=CARTESIAN_POINT('Ctrl Pts',(7.65868976978871,-18.6280491346907,21.));
#9271=CARTESIAN_POINT('Ctrl Pts',(7.65741532450727,-18.5788385228928,0.));
#9272=CARTESIAN_POINT('Ctrl Pts',(7.65741532450727,-18.5788385228928,21.));
#9273=CARTESIAN_POINT('Ctrl Pts',(7.65580722110436,-18.5297146894905,0.));
#9274=CARTESIAN_POINT('Ctrl Pts',(7.65580722110436,-18.5297146894905,21.));
#9275=CARTESIAN_POINT('Ctrl Pts',(7.65386603444742,-18.4806785483052,0.));
#9276=CARTESIAN_POINT('Ctrl Pts',(7.65386603444742,-18.4806785483052,21.));
#9277=CARTESIAN_POINT('Ctrl Pts',(7.65158974829126,-18.4317319183719,0.));
#9278=CARTESIAN_POINT('Ctrl Pts',(7.65158974829126,-18.4317319183719,21.));
#9279=CARTESIAN_POINT('Ctrl Pts',(7.6489719793775,-18.3828781275628,0.));
#9280=CARTESIAN_POINT('Ctrl Pts',(7.6489719793775,-18.3828781275628,21.));
#9281=CARTESIAN_POINT('Ctrl Pts',(7.64599903846601,-18.3341230095852,0.));
#9282=CARTESIAN_POINT('Ctrl Pts',(7.64599903846601,-18.3341230095852,21.));
#9283=CARTESIAN_POINT('Ctrl Pts',(7.64265220270759,-18.2854741391282,0.));
#9284=CARTESIAN_POINT('Ctrl Pts',(7.64265220270759,-18.2854741391282,21.));
#9285=CARTESIAN_POINT('Ctrl Pts',(7.63891299603826,-18.2369390502576,0.));
#9286=CARTESIAN_POINT('Ctrl Pts',(7.63891299603826,-18.2369390502576,21.));
#9287=CARTESIAN_POINT('Ctrl Pts',(7.63476798969016,-18.1885236169197,0.));
#9288=CARTESIAN_POINT('Ctrl Pts',(7.63476798969016,-18.1885236169197,21.));
#9289=CARTESIAN_POINT('Ctrl Pts',(7.63021285851761,-18.1402306858819,0.));
#9290=CARTESIAN_POINT('Ctrl Pts',(7.63021285851761,-18.1402306858819,21.));
#9291=CARTESIAN_POINT('Ctrl Pts',(7.62525915358073,-18.0920577897363,0.));
#9292=CARTESIAN_POINT('Ctrl Pts',(7.62525915358073,-18.0920577897363,21.));
#9293=CARTESIAN_POINT('Ctrl Pts',(7.61992799636653,-18.0439992897906,0.));
#9294=CARTESIAN_POINT('Ctrl Pts',(7.61992799636653,-18.0439992897906,21.));
#9295=CARTESIAN_POINT('Ctrl Pts',(7.61423755067037,-17.9960506269561,0.));
#9296=CARTESIAN_POINT('Ctrl Pts',(7.61423755067037,-17.9960506269561,21.));
#9297=CARTESIAN_POINT('Ctrl Pts',(7.60819152580111,-17.9482122228183,0.));
#9298=CARTESIAN_POINT('Ctrl Pts',(7.60819152580111,-17.9482122228183,21.));
#9299=CARTESIAN_POINT('Ctrl Pts',(7.60176928403058,-17.900492838997,0.));
#9300=CARTESIAN_POINT('Ctrl Pts',(7.60176928403058,-17.900492838997,21.));
#9301=CARTESIAN_POINT('Ctrl Pts',(7.59491004201955,-17.8529149331931,0.));
#9302=CARTESIAN_POINT('Ctrl Pts',(7.59491004201955,-17.8529149331931,21.));
#9303=CARTESIAN_POINT('Ctrl Pts',(7.58752955799498,-17.8055090348024,0.));
#9304=CARTESIAN_POINT('Ctrl Pts',(7.58752955799498,-17.8055090348024,21.));
#9305=CARTESIAN_POINT('Ctrl Pts',(7.57954834582803,-17.7583042294209,0.));
#9306=CARTESIAN_POINT('Ctrl Pts',(7.57954834582803,-17.7583042294209,21.));
#9307=CARTESIAN_POINT('Ctrl Pts',(7.57091795530423,-17.7113192869136,0.));
#9308=CARTESIAN_POINT('Ctrl Pts',(7.57091795530423,-17.7113192869136,21.));
#9309=CARTESIAN_POINT('Ctrl Pts',(7.56164400295862,-17.6645549117314,0.));
#9310=CARTESIAN_POINT('Ctrl Pts',(7.56164400295862,-17.6645549117314,21.));
#9311=CARTESIAN_POINT('Ctrl Pts',(7.55182125346563,-17.6179818599248,0.));
#9312=CARTESIAN_POINT('Ctrl Pts',(7.55182125346563,-17.6179818599248,21.));
#9313=CARTESIAN_POINT('Ctrl Pts',(7.54158441095317,-17.5715579419204,0.));
#9314=CARTESIAN_POINT('Ctrl Pts',(7.54158441095317,-17.5715579419204,21.));
#9315=CARTESIAN_POINT('Ctrl Pts',(7.53103903007863,-17.5252518287336,0.));
#9316=CARTESIAN_POINT('Ctrl Pts',(7.53103903007863,-17.5252518287336,21.));
#9317=CARTESIAN_POINT('Ctrl Pts',(7.52019696747328,-17.4790653226646,0.));
#9318=CARTESIAN_POINT('Ctrl Pts',(7.52019696747328,-17.4790653226646,21.));
#9319=CARTESIAN_POINT('Ctrl Pts',(7.50891486634214,-17.4330545448126,0.));
#9320=CARTESIAN_POINT('Ctrl Pts',(7.50891486634214,-17.4330545448126,21.));
#9321=CARTESIAN_POINT('Ctrl Pts',(7.4968177445175,-17.3873563447297,0.));
#9322=CARTESIAN_POINT('Ctrl Pts',(7.4968177445175,-17.3873563447297,21.));
#9323=CARTESIAN_POINT('Ctrl Pts',(7.48340100912745,-17.3421522689127,0.));
#9324=CARTESIAN_POINT('Ctrl Pts',(7.48340100912745,-17.3421522689127,21.));
#9325=CARTESIAN_POINT('Ctrl Pts',(7.47120323460919,-17.3065305096784,0.));
#9326=CARTESIAN_POINT('Ctrl Pts',(7.47120323460919,-17.3065305096784,21.));
#9327=CARTESIAN_POINT('Ctrl Pts',(7.4610504981825,-17.2801832097582,0.));
#9328=CARTESIAN_POINT('Ctrl Pts',(7.4610504981825,-17.2801832097582,21.));
#9329=CARTESIAN_POINT('Ctrl Pts',(7.45381253347182,-17.2627905583523,0.));
#9330=CARTESIAN_POINT('Ctrl Pts',(7.45381253347182,-17.2627905583523,21.));
#9331=CARTESIAN_POINT('Ctrl Pts',(7.45007618140238,-17.2541372868972,0.));
#9332=CARTESIAN_POINT('Ctrl Pts',(7.45007618140238,-17.2541372868972,21.));
#9333=CARTESIAN_POINT('',(7.45574324794406,-20.698113262342,0.));
#9334=CARTESIAN_POINT('Ctrl Pts',(7.45007618140238,-17.2541372868972,0.));
#9335=CARTESIAN_POINT('Ctrl Pts',(7.45381253347182,-17.2627905583523,0.));
#9336=CARTESIAN_POINT('Ctrl Pts',(7.4610504981825,-17.2801832097582,0.));
#9337=CARTESIAN_POINT('Ctrl Pts',(7.47120323460919,-17.3065305096784,0.));
#9338=CARTESIAN_POINT('Ctrl Pts',(7.48340100912745,-17.3421522689127,0.));
#9339=CARTESIAN_POINT('Ctrl Pts',(7.4968177445175,-17.3873563447297,0.));
#9340=CARTESIAN_POINT('Ctrl Pts',(7.50891486634214,-17.4330545448126,0.));
#9341=CARTESIAN_POINT('Ctrl Pts',(7.52019696747328,-17.4790653226646,0.));
#9342=CARTESIAN_POINT('Ctrl Pts',(7.53103903007863,-17.5252518287336,0.));
#9343=CARTESIAN_POINT('Ctrl Pts',(7.54158441095317,-17.5715579419204,0.));
#9344=CARTESIAN_POINT('Ctrl Pts',(7.55182125346563,-17.6179818599248,0.));
#9345=CARTESIAN_POINT('Ctrl Pts',(7.56164400295862,-17.6645549117314,0.));
#9346=CARTESIAN_POINT('Ctrl Pts',(7.57091795530423,-17.7113192869136,0.));
#9347=CARTESIAN_POINT('Ctrl Pts',(7.57954834582803,-17.7583042294209,0.));
#9348=CARTESIAN_POINT('Ctrl Pts',(7.58752955799498,-17.8055090348024,0.));
#9349=CARTESIAN_POINT('Ctrl Pts',(7.59491004201955,-17.8529149331931,0.));
#9350=CARTESIAN_POINT('Ctrl Pts',(7.60176928403058,-17.900492838997,0.));
#9351=CARTESIAN_POINT('Ctrl Pts',(7.60819152580111,-17.9482122228183,0.));
#9352=CARTESIAN_POINT('Ctrl Pts',(7.61423755067037,-17.9960506269561,0.));
#9353=CARTESIAN_POINT('Ctrl Pts',(7.61992799636653,-18.0439992897906,0.));
#9354=CARTESIAN_POINT('Ctrl Pts',(7.62525915358073,-18.0920577897363,0.));
#9355=CARTESIAN_POINT('Ctrl Pts',(7.63021285851761,-18.1402306858819,0.));
#9356=CARTESIAN_POINT('Ctrl Pts',(7.63476798969016,-18.1885236169197,0.));
#9357=CARTESIAN_POINT('Ctrl Pts',(7.63891299603826,-18.2369390502576,0.));
#9358=CARTESIAN_POINT('Ctrl Pts',(7.64265220270759,-18.2854741391282,0.));
#9359=CARTESIAN_POINT('Ctrl Pts',(7.64599903846601,-18.3341230095852,0.));
#9360=CARTESIAN_POINT('Ctrl Pts',(7.6489719793775,-18.3828781275628,0.));
#9361=CARTESIAN_POINT('Ctrl Pts',(7.65158974829126,-18.4317319183719,0.));
#9362=CARTESIAN_POINT('Ctrl Pts',(7.65386603444742,-18.4806785483052,0.));
#9363=CARTESIAN_POINT('Ctrl Pts',(7.65580722110436,-18.5297146894905,0.));
#9364=CARTESIAN_POINT('Ctrl Pts',(7.65741532450727,-18.5788385228928,0.));
#9365=CARTESIAN_POINT('Ctrl Pts',(7.65868976978871,-18.6280491346907,0.));
#9366=CARTESIAN_POINT('Ctrl Pts',(7.65962948375621,-18.6773458057584,0.));
#9367=CARTESIAN_POINT('Ctrl Pts',(7.66023521705904,-18.7267272235231,0.));
#9368=CARTESIAN_POINT('Ctrl Pts',(7.6605104692254,-18.7761911671591,0.));
#9369=CARTESIAN_POINT('Ctrl Pts',(7.66046025294774,-18.8257349246207,0.));
#9370=CARTESIAN_POINT('Ctrl Pts',(7.66009036321662,-18.8753555389435,0.));
#9371=CARTESIAN_POINT('Ctrl Pts',(7.65940650980098,-18.9250501008887,0.));
#9372=CARTESIAN_POINT('Ctrl Pts',(7.65841335587266,-18.974816073814,0.));
#9373=CARTESIAN_POINT('Ctrl Pts',(7.65711415727854,-19.0246514144531,0.));
#9374=CARTESIAN_POINT('Ctrl Pts',(7.65551129907201,-19.0745543888799,0.));
#9375=CARTESIAN_POINT('Ctrl Pts',(7.65360662280608,-19.1245234597312,0.));
#9376=CARTESIAN_POINT('Ctrl Pts',(7.65140181220525,-19.1745571539291,0.));
#9377=CARTESIAN_POINT('Ctrl Pts',(7.64889882291923,-19.224653915265,0.));
#9378=CARTESIAN_POINT('Ctrl Pts',(7.64610005549613,-19.2748120456486,0.));
#9379=CARTESIAN_POINT('Ctrl Pts',(7.64300812875338,-19.3250297839295,0.));
#9380=CARTESIAN_POINT('Ctrl Pts',(7.6396257482276,-19.3753053524647,0.));
#9381=CARTESIAN_POINT('Ctrl Pts',(7.63595554930653,-19.4256370121006,0.));
#9382=CARTESIAN_POINT('Ctrl Pts',(7.63199992715365,-19.4760231231881,0.));
#9383=CARTESIAN_POINT('Ctrl Pts',(7.62776096538882,-19.5264621687521,0.));
#9384=CARTESIAN_POINT('Ctrl Pts',(7.62324053735219,-19.5769527121826,0.));
#9385=CARTESIAN_POINT('Ctrl Pts',(7.6184403707059,-19.6274933688524,0.));
#9386=CARTESIAN_POINT('Ctrl Pts',(7.61336212350878,-19.6780827744426,0.));
#9387=CARTESIAN_POINT('Ctrl Pts',(7.60800746969261,-19.7287195480601,0.));
#9388=CARTESIAN_POINT('Ctrl Pts',(7.60237814110186,-19.7794022782484,0.));
#9389=CARTESIAN_POINT('Ctrl Pts',(7.59647587605448,-19.830129556152,0.));
#9390=CARTESIAN_POINT('Ctrl Pts',(7.59030238888851,-19.8808999994024,0.));
#9391=CARTESIAN_POINT('Ctrl Pts',(7.58385933533351,-19.931712276832,0.));
#9392=CARTESIAN_POINT('Ctrl Pts',(7.57714827622805,-19.9825651387294,0.));
#9393=CARTESIAN_POINT('Ctrl Pts',(7.57017066105972,-20.0334574248557,0.));
#9394=CARTESIAN_POINT('Ctrl Pts',(7.5629278654946,-20.0843880130978,0.));
#9395=CARTESIAN_POINT('Ctrl Pts',(7.55542122125494,-20.1353557774357,0.));
#9396=CARTESIAN_POINT('Ctrl Pts',(7.54765204869254,-20.1863595454674,0.));
#9397=CARTESIAN_POINT('Ctrl Pts',(7.53962169534166,-20.2373980474879,0.));
#9398=CARTESIAN_POINT('Ctrl Pts',(7.53133155804007,-20.2884698940944,0.));
#9399=CARTESIAN_POINT('Ctrl Pts',(7.52278303006887,-20.3395736743243,0.));
#9400=CARTESIAN_POINT('Ctrl Pts',(7.51397746081993,-20.3907080367098,0.));
#9401=CARTESIAN_POINT('Ctrl Pts',(7.50491611266253,-20.4418717748497,0.));
#9402=CARTESIAN_POINT('Ctrl Pts',(7.49560012018405,-20.4930639156161,0.));
#9403=CARTESIAN_POINT('Ctrl Pts',(7.48411651832412,-20.5545277683621,0.));
#9404=CARTESIAN_POINT('Ctrl Pts',(7.47423073598681,-20.6057817877246,0.));
#9405=CARTESIAN_POINT('Ctrl Pts',(7.46612041736313,-20.6468066077586,0.));
#9406=CARTESIAN_POINT('Ctrl Pts',(7.45992433946823,-20.6775873630604,0.));
#9407=CARTESIAN_POINT('Ctrl Pts',(7.455743247944,-20.698113262342,0.));
#9408=CARTESIAN_POINT('',(7.45574324794406,-20.698113262342,13.));
#9409=CARTESIAN_POINT('Ctrl Pts',(7.455743247944,-20.698113262342,13.));
#9410=CARTESIAN_POINT('Ctrl Pts',(7.47632490106067,-20.5970733933809,13.));
#9411=CARTESIAN_POINT('Ctrl Pts',(7.49544541955086,-20.496187784905,13.));
#9412=CARTESIAN_POINT('Ctrl Pts',(7.51308219823822,-20.3954689842507,13.));
#9413=CARTESIAN_POINT('Ctrl Pts',(7.54230710648616,-20.2285735573624,13.));
#9414=CARTESIAN_POINT('Ctrl Pts',(7.56745095675757,-20.0621477318166,13.));
#9415=CARTESIAN_POINT('Ctrl Pts',(7.58830059897784,-19.8963869129096,13.));
#9416=CARTESIAN_POINT('Ctrl Pts',(7.60432685672297,-19.7689734263959,13.));
#9417=CARTESIAN_POINT('Ctrl Pts',(7.6178148542035,-19.6419503944581,13.));
#9418=CARTESIAN_POINT('Ctrl Pts',(7.62864367929131,-19.5154161645489,13.));
#9419=CARTESIAN_POINT('Ctrl Pts',(7.64030064883062,-19.3792051119398,13.));
#9420=CARTESIAN_POINT('Ctrl Pts',(7.64888186436128,-19.2435576445087,13.));
#9421=CARTESIAN_POINT('Ctrl Pts',(7.65417053742034,-19.1086228836098,13.));
#9422=CARTESIAN_POINT('Ctrl Pts',(7.6570984904104,-19.0339193365717,13.));
#9423=CARTESIAN_POINT('Ctrl Pts',(7.65902218171088,-18.9594327324131,13.));
#9424=CARTESIAN_POINT('Ctrl Pts',(7.65990167998048,-18.8851905418284,13.));
#9425=CARTESIAN_POINT('Ctrl Pts',(7.66074919903795,-18.8136478525884,13.));
#9426=CARTESIAN_POINT('Ctrl Pts',(7.66062065572298,-18.7423342828967,13.));
#9427=CARTESIAN_POINT('Ctrl Pts',(7.65944821270055,-18.6712863090049,13.));
#9428=CARTESIAN_POINT('Ctrl Pts',(7.65843486239164,-18.6098790722244,13.));
#9429=CARTESIAN_POINT('Ctrl Pts',(7.65664478982407,-18.5486691991956,13.));
#9430=CARTESIAN_POINT('Ctrl Pts',(7.65407864069922,-18.4876659849921,13.));
#9431=CARTESIAN_POINT('Ctrl Pts',(7.6522370315769,-18.4438867382289,13.));
#9432=CARTESIAN_POINT('Ctrl Pts',(7.64999840197462,-18.4002130327578,13.));
#9433=CARTESIAN_POINT('Ctrl Pts',(7.6473265656267,-18.3566609384042,13.));
#9434=CARTESIAN_POINT('Ctrl Pts',(7.6446982368131,-18.3138180357798,13.));
#9435=CARTESIAN_POINT('Ctrl Pts',(7.64164464439788,-18.2710948572858,13.));
#9436=CARTESIAN_POINT('Ctrl Pts',(7.63811742043929,-18.2285117407612,13.));
#9437=CARTESIAN_POINT('Ctrl Pts',(7.63505911004306,-18.1915896769798,13.));
#9438=CARTESIAN_POINT('Ctrl Pts',(7.63164238136018,-18.1547737064202,13.));
#9439=CARTESIAN_POINT('Ctrl Pts',(7.62788266165966,-18.1180614604294,13.));
#9440=CARTESIAN_POINT('Ctrl Pts',(7.62447721821563,-18.0848085885711,13.));
#9441=CARTESIAN_POINT('Ctrl Pts',(7.62079564900185,-18.0516390296195,13.));
#9442=CARTESIAN_POINT('Ctrl Pts',(7.61686093607235,-18.0185473584385,13.));
#9443=CARTESIAN_POINT('Ctrl Pts',(7.613546541745,-17.9906726826464,13.));
#9444=CARTESIAN_POINT('Ctrl Pts',(7.61005417561771,-17.9628527173707,13.));
#9445=CARTESIAN_POINT('Ctrl Pts',(7.60636550500381,-17.9350952312728,13.));
#9446=CARTESIAN_POINT('Ctrl Pts',(7.60102759729104,-17.8949271288214,13.));
#9447=CARTESIAN_POINT('Ctrl Pts',(7.59527782596877,-17.8548900767427,13.));
#9448=CARTESIAN_POINT('Ctrl Pts',(7.58891067826389,-17.8150590779995,13.));
#9449=CARTESIAN_POINT('Ctrl Pts',(7.58506340059934,-17.7909916432666,13.));
#9450=CARTESIAN_POINT('Ctrl Pts',(7.58098742040086,-17.7670005718324,13.));
#9451=CARTESIAN_POINT('Ctrl Pts',(7.57665817621866,-17.7430955913955,13.));
#9452=CARTESIAN_POINT('Ctrl Pts',(7.57266539519107,-17.7210484745465,13.));
#9453=CARTESIAN_POINT('Ctrl Pts',(7.56845593268894,-17.6990750119179,13.));
#9454=CARTESIAN_POINT('Ctrl Pts',(7.5640539035508,-17.677168309485,13.));
#9455=CARTESIAN_POINT('Ctrl Pts',(7.55799846635133,-17.6470334201721,13.));
#9456=CARTESIAN_POINT('Ctrl Pts',(7.55158552707213,-17.6170224065982,13.));
#9457=CARTESIAN_POINT('Ctrl Pts',(7.54495919885622,-17.5870909089353,13.));
#9458=CARTESIAN_POINT('Ctrl Pts',(7.54075533803913,-17.5681018329159,13.));
#9459=CARTESIAN_POINT('Ctrl Pts',(7.53646718585673,-17.5491442490901,13.));
#9460=CARTESIAN_POINT('Ctrl Pts',(7.53210330803199,-17.5302169633181,13.));
#9461=CARTESIAN_POINT('Ctrl Pts',(7.52818693080402,-17.5132306053213,13.));
#9462=CARTESIAN_POINT('Ctrl Pts',(7.52421025221346,-17.4962684160965,13.));
#9463=CARTESIAN_POINT('Ctrl Pts',(7.5201410653043,-17.4793429835169,13.));
#9464=CARTESIAN_POINT('Ctrl Pts',(7.51586353943418,-17.4615509829677,13.));
#9465=CARTESIAN_POINT('Ctrl Pts',(7.51148394209619,-17.4437995539328,13.));
#9466=CARTESIAN_POINT('Ctrl Pts',(7.506906015607,-17.4261238143115,13.));
#9467=CARTESIAN_POINT('Ctrl Pts',(7.49930208984073,-17.3967644499221,13.));
#9468=CARTESIAN_POINT('Ctrl Pts',(7.49114308213723,-17.3676168188804,13.));
#9469=CARTESIAN_POINT('Ctrl Pts',(7.48183975621879,-17.3388922514903,13.));
#9470=CARTESIAN_POINT('Ctrl Pts',(7.47670957121225,-17.3230525027557,13.));
#9471=CARTESIAN_POINT('Ctrl Pts',(7.47123011545282,-17.3073418194655,13.));
#9472=CARTESIAN_POINT('Ctrl Pts',(7.46532888198223,-17.2917860605788,13.));
#9473=CARTESIAN_POINT('Ctrl Pts',(7.46052853291189,-17.2791322530176,13.));
#9474=CARTESIAN_POINT('Ctrl Pts',(7.45544915949247,-17.2665809316801,13.));
#9475=CARTESIAN_POINT('Ctrl Pts',(7.45007618140238,-17.2541372868972,13.));
#9476=CARTESIAN_POINT('',(7.45574324794406,-20.698113262342,0.));
#9477=CARTESIAN_POINT('Origin',(1.75106900012182E-12,-5.38923623413286E-12,
0.));
#9478=CARTESIAN_POINT('',(6.1342227326009,-21.1275013067528,0.));
#9479=CARTESIAN_POINT('Origin',(1.75106900012182E-12,-5.38923623413286E-12,
0.));
#9480=CARTESIAN_POINT('',(6.1342227326009,-21.1275013067528,13.));
#9481=CARTESIAN_POINT('Origin',(1.75106900012182E-12,-5.38923623413286E-12,
13.));
#9482=CARTESIAN_POINT('',(6.1342227326009,-21.1275013067528,0.));
#9483=CARTESIAN_POINT('Ctrl Pts',(4.1144891981253,-18.337935196262,0.));
#9484=CARTESIAN_POINT('Ctrl Pts',(4.1144891981253,-18.337935196262,21.));
#9485=CARTESIAN_POINT('Ctrl Pts',(4.11655269114951,-18.3471320125699,0.));
#9486=CARTESIAN_POINT('Ctrl Pts',(4.11655269114951,-18.3471320125699,21.));
#9487=CARTESIAN_POINT('Ctrl Pts',(4.12092019868859,-18.3654573320481,0.));
#9488=CARTESIAN_POINT('Ctrl Pts',(4.12092019868859,-18.3654573320481,21.));
#9489=CARTESIAN_POINT('Ctrl Pts',(4.12819301671078,-18.3927403741815,0.));
#9490=CARTESIAN_POINT('Ctrl Pts',(4.12819301671078,-18.3927403741815,21.));
#9491=CARTESIAN_POINT('Ctrl Pts',(4.13926275457062,-18.4287286547442,0.));
#9492=CARTESIAN_POINT('Ctrl Pts',(4.13926275457062,-18.4287286547442,21.));
#9493=CARTESIAN_POINT('Ctrl Pts',(4.15497867673974,-18.4731856794913,0.));
#9494=CARTESIAN_POINT('Ctrl Pts',(4.15497867673974,-18.4731856794913,21.));
#9495=CARTESIAN_POINT('Ctrl Pts',(4.17205262766561,-18.5172668097744,0.));
#9496=CARTESIAN_POINT('Ctrl Pts',(4.17205262766561,-18.5172668097744,21.));
#9497=CARTESIAN_POINT('Ctrl Pts',(4.1899696727862,-18.5611217636409,0.));
#9498=CARTESIAN_POINT('Ctrl Pts',(4.1899696727862,-18.5611217636409,21.));
#9499=CARTESIAN_POINT('Ctrl Pts',(4.20834600700664,-18.6048602364653,0.));
#9500=CARTESIAN_POINT('Ctrl Pts',(4.20834600700664,-18.6048602364653,21.));
#9501=CARTESIAN_POINT('Ctrl Pts',(4.22703266508918,-18.6485210883348,0.));
#9502=CARTESIAN_POINT('Ctrl Pts',(4.22703266508918,-18.6485210883348,21.));
#9503=CARTESIAN_POINT('Ctrl Pts',(4.24603817988452,-18.6920958920047,0.));
#9504=CARTESIAN_POINT('Ctrl Pts',(4.24603817988452,-18.6920958920047,21.));
#9505=CARTESIAN_POINT('Ctrl Pts',(4.26546636161932,-18.735547949685,0.));
#9506=CARTESIAN_POINT('Ctrl Pts',(4.26546636161932,-18.735547949685,21.));
#9507=CARTESIAN_POINT('Ctrl Pts',(4.28545098663152,-18.778832216358,0.));
#9508=CARTESIAN_POINT('Ctrl Pts',(4.28545098663152,-18.778832216358,21.));
#9509=CARTESIAN_POINT('Ctrl Pts',(4.30608591031525,-18.8219166495975,0.));
#9510=CARTESIAN_POINT('Ctrl Pts',(4.30608591031525,-18.8219166495975,21.));
#9511=CARTESIAN_POINT('Ctrl Pts',(4.32737526247704,-18.8647973781745,0.));
#9512=CARTESIAN_POINT('Ctrl Pts',(4.32737526247704,-18.8647973781745,21.));
#9513=CARTESIAN_POINT('Ctrl Pts',(4.34926881342021,-18.9074876952706,0.));
#9514=CARTESIAN_POINT('Ctrl Pts',(4.34926881342021,-18.9074876952706,21.));
#9515=CARTESIAN_POINT('Ctrl Pts',(4.37168516143122,-18.9500107909187,0.));
#9516=CARTESIAN_POINT('Ctrl Pts',(4.37168516143122,-18.9500107909187,21.));
#9517=CARTESIAN_POINT('Ctrl Pts',(4.39453820875554,-18.9923914823906,0.));
#9518=CARTESIAN_POINT('Ctrl Pts',(4.39453820875554,-18.9923914823906,21.));
#9519=CARTESIAN_POINT('Ctrl Pts',(4.41776558033331,-19.034647328575,0.));
#9520=CARTESIAN_POINT('Ctrl Pts',(4.41776558033331,-19.034647328575,21.));
#9521=CARTESIAN_POINT('Ctrl Pts',(4.44134542994081,-19.0767833717249,0.));
#9522=CARTESIAN_POINT('Ctrl Pts',(4.44134542994081,-19.0767833717249,21.));
#9523=CARTESIAN_POINT('Ctrl Pts',(4.46528051067021,-19.1187970904933,0.));
#9524=CARTESIAN_POINT('Ctrl Pts',(4.46528051067021,-19.1187970904933,21.));
#9525=CARTESIAN_POINT('Ctrl Pts',(4.48958819710576,-19.1606814968494,0.));
#9526=CARTESIAN_POINT('Ctrl Pts',(4.48958819710576,-19.1606814968494,21.));
#9527=CARTESIAN_POINT('Ctrl Pts',(4.51428889122954,-19.2024287376926,0.));
#9528=CARTESIAN_POINT('Ctrl Pts',(4.51428889122954,-19.2024287376926,21.));
#9529=CARTESIAN_POINT('Ctrl Pts',(4.53939338835151,-19.2440340196551,0.));
#9530=CARTESIAN_POINT('Ctrl Pts',(4.53939338835151,-19.2440340196551,21.));
#9531=CARTESIAN_POINT('Ctrl Pts',(4.5648965160674,-19.2854975819105,0.));
#9532=CARTESIAN_POINT('Ctrl Pts',(4.5648965160674,-19.2854975819105,21.));
#9533=CARTESIAN_POINT('Ctrl Pts',(4.59078395765677,-19.3268225655679,0.));
#9534=CARTESIAN_POINT('Ctrl Pts',(4.59078395765677,-19.3268225655679,21.));
#9535=CARTESIAN_POINT('Ctrl Pts',(4.61703633725711,-19.3680137353983,0.));
#9536=CARTESIAN_POINT('Ctrl Pts',(4.61703633725711,-19.3680137353983,21.));
#9537=CARTESIAN_POINT('Ctrl Pts',(4.64363405547472,-19.4090759683639,0.));
#9538=CARTESIAN_POINT('Ctrl Pts',(4.64363405547472,-19.4090759683639,21.));
#9539=CARTESIAN_POINT('Ctrl Pts',(4.67056260851452,-19.4500125912299,0.));
#9540=CARTESIAN_POINT('Ctrl Pts',(4.67056260851452,-19.4500125912299,21.));
#9541=CARTESIAN_POINT('Ctrl Pts',(4.69781487613784,-19.4908246636763,0.));
#9542=CARTESIAN_POINT('Ctrl Pts',(4.69781487613784,-19.4908246636763,21.));
#9543=CARTESIAN_POINT('Ctrl Pts',(4.72538815796615,-19.531511899192,0.));
#9544=CARTESIAN_POINT('Ctrl Pts',(4.72538815796615,-19.531511899192,21.));
#9545=CARTESIAN_POINT('Ctrl Pts',(4.7532823819461,-19.5720732205813,0.));
#9546=CARTESIAN_POINT('Ctrl Pts',(4.7532823819461,-19.5720732205813,21.));
#9547=CARTESIAN_POINT('Ctrl Pts',(4.7814979936173,-19.6125074152527,0.));
#9548=CARTESIAN_POINT('Ctrl Pts',(4.7814979936173,-19.6125074152527,21.));
#9549=CARTESIAN_POINT('Ctrl Pts',(4.8100336141806,-19.6528138625329,0.));
#9550=CARTESIAN_POINT('Ctrl Pts',(4.8100336141806,-19.6528138625329,21.));
#9551=CARTESIAN_POINT('Ctrl Pts',(4.83888510708974,-19.6929928227072,0.));
#9552=CARTESIAN_POINT('Ctrl Pts',(4.83888510708974,-19.6929928227072,21.));
#9553=CARTESIAN_POINT('Ctrl Pts',(4.86804682289086,-19.7330450480715,0.));
#9554=CARTESIAN_POINT('Ctrl Pts',(4.86804682289086,-19.7330450480715,21.));
#9555=CARTESIAN_POINT('Ctrl Pts',(4.89751233527804,-19.772971552601,0.));
#9556=CARTESIAN_POINT('Ctrl Pts',(4.89751233527804,-19.772971552601,21.));
#9557=CARTESIAN_POINT('Ctrl Pts',(4.92727531494346,-19.8127733387903,0.));
#9558=CARTESIAN_POINT('Ctrl Pts',(4.92727531494346,-19.8127733387903,21.));
#9559=CARTESIAN_POINT('Ctrl Pts',(4.95733049830095,-19.8524510953961,0.));
#9560=CARTESIAN_POINT('Ctrl Pts',(4.95733049830095,-19.8524510953961,21.));
#9561=CARTESIAN_POINT('Ctrl Pts',(4.98767405031333,-19.8920050831202,0.));
#9562=CARTESIAN_POINT('Ctrl Pts',(4.98767405031333,-19.8920050831202,21.));
#9563=CARTESIAN_POINT('Ctrl Pts',(5.01830302225557,-19.931435301086,0.));
#9564=CARTESIAN_POINT('Ctrl Pts',(5.01830302225557,-19.931435301086,21.));
#9565=CARTESIAN_POINT('Ctrl Pts',(5.04921502064063,-19.9707415879783,0.));
#9566=CARTESIAN_POINT('Ctrl Pts',(5.04921502064063,-19.9707415879783,21.));
#9567=CARTESIAN_POINT('Ctrl Pts',(5.08040781745336,-20.0099237417205,0.));
#9568=CARTESIAN_POINT('Ctrl Pts',(5.08040781745336,-20.0099237417205,21.));
#9569=CARTESIAN_POINT('Ctrl Pts',(5.11187891582334,-20.0489816528155,0.));
#9570=CARTESIAN_POINT('Ctrl Pts',(5.11187891582334,-20.0489816528155,21.));
#9571=CARTESIAN_POINT('Ctrl Pts',(5.14362537555397,-20.087915358486,0.));
#9572=CARTESIAN_POINT('Ctrl Pts',(5.14362537555397,-20.087915358486,21.));
#9573=CARTESIAN_POINT('Ctrl Pts',(5.17564404279921,-20.1267249732337,0.));
#9574=CARTESIAN_POINT('Ctrl Pts',(5.17564404279921,-20.1267249732337,21.));
#9575=CARTESIAN_POINT('Ctrl Pts',(5.20793168386163,-20.1654106491899,0.));
#9576=CARTESIAN_POINT('Ctrl Pts',(5.20793168386163,-20.1654106491899,21.));
#9577=CARTESIAN_POINT('Ctrl Pts',(5.2404851444189,-20.2039725283917,0.));
#9578=CARTESIAN_POINT('Ctrl Pts',(5.2404851444189,-20.2039725283917,21.));
#9579=CARTESIAN_POINT('Ctrl Pts',(5.27330152298149,-20.2424106921768,0.));
#9580=CARTESIAN_POINT('Ctrl Pts',(5.27330152298149,-20.2424106921768,21.));
#9581=CARTESIAN_POINT('Ctrl Pts',(5.30637824220997,-20.2807251380077,0.));
#9582=CARTESIAN_POINT('Ctrl Pts',(5.30637824220997,-20.2807251380077,21.));
#9583=CARTESIAN_POINT('Ctrl Pts',(5.33971294212213,-20.3189158047642,0.));
#9584=CARTESIAN_POINT('Ctrl Pts',(5.33971294212213,-20.3189158047642,21.));
#9585=CARTESIAN_POINT('Ctrl Pts',(5.37330341114648,-20.3569825877537,0.));
#9586=CARTESIAN_POINT('Ctrl Pts',(5.37330341114648,-20.3569825877537,21.));
#9587=CARTESIAN_POINT('Ctrl Pts',(5.40714750595874,-20.3949253578015,0.));
#9588=CARTESIAN_POINT('Ctrl Pts',(5.40714750595874,-20.3949253578015,21.));
#9589=CARTESIAN_POINT('Ctrl Pts',(5.4412430606511,-20.4327439816542,0.));
#9590=CARTESIAN_POINT('Ctrl Pts',(5.4412430606511,-20.4327439816542,21.));
#9591=CARTESIAN_POINT('Ctrl Pts',(5.4755878444985,-20.4704383353718,0.));
#9592=CARTESIAN_POINT('Ctrl Pts',(5.4755878444985,-20.4704383353718,21.));
#9593=CARTESIAN_POINT('Ctrl Pts',(5.51017962306782,-20.5080083009242,0.));
#9594=CARTESIAN_POINT('Ctrl Pts',(5.51017962306782,-20.5080083009242,21.));
#9595=CARTESIAN_POINT('Ctrl Pts',(5.54501619689459,-20.5454537676144,0.));
#9596=CARTESIAN_POINT('Ctrl Pts',(5.54501619689459,-20.5454537676144,21.));
#9597=CARTESIAN_POINT('Ctrl Pts',(5.58009544402474,-20.5827746317185,0.));
#9598=CARTESIAN_POINT('Ctrl Pts',(5.58009544402474,-20.5827746317185,21.));
#9599=CARTESIAN_POINT('Ctrl Pts',(5.61541536715148,-20.6199707996366,0.));
#9600=CARTESIAN_POINT('Ctrl Pts',(5.61541536715148,-20.6199707996366,21.));
#9601=CARTESIAN_POINT('Ctrl Pts',(5.65097411164334,-20.6570421847033,0.));
#9602=CARTESIAN_POINT('Ctrl Pts',(5.65097411164334,-20.6570421847033,21.));
#9603=CARTESIAN_POINT('Ctrl Pts',(5.68676990500163,-20.6939886877061,0.));
#9604=CARTESIAN_POINT('Ctrl Pts',(5.68676990500163,-20.6939886877061,21.));
#9605=CARTESIAN_POINT('Ctrl Pts',(5.7228010079824,-20.7308101804425,0.));
#9606=CARTESIAN_POINT('Ctrl Pts',(5.7228010079824,-20.7308101804425,21.));
#9607=CARTESIAN_POINT('Ctrl Pts',(5.75906566327795,-20.7675064905026,0.));
#9608=CARTESIAN_POINT('Ctrl Pts',(5.75906566327795,-20.7675064905026,21.));
#9609=CARTESIAN_POINT('Ctrl Pts',(5.79556203439643,-20.8040773827343,0.));
#9610=CARTESIAN_POINT('Ctrl Pts',(5.79556203439643,-20.8040773827343,21.));
#9611=CARTESIAN_POINT('Ctrl Pts',(5.83228817460177,-20.8405225541277,0.));
#9612=CARTESIAN_POINT('Ctrl Pts',(5.83228817460177,-20.8405225541277,21.));
#9613=CARTESIAN_POINT('Ctrl Pts',(5.86924212736287,-20.8768416821402,0.));
#9614=CARTESIAN_POINT('Ctrl Pts',(5.86924212736287,-20.8768416821402,21.));
#9615=CARTESIAN_POINT('Ctrl Pts',(5.90642200662599,-20.9130344665641,0.));
#9616=CARTESIAN_POINT('Ctrl Pts',(5.90642200662599,-20.9130344665641,21.));
#9617=CARTESIAN_POINT('Ctrl Pts',(5.94382608200804,-20.9491006734021,0.));
#9618=CARTESIAN_POINT('Ctrl Pts',(5.94382608200804,-20.9491006734021,21.));
#9619=CARTESIAN_POINT('Ctrl Pts',(5.98145286361836,-20.9850401822713,0.));
#9620=CARTESIAN_POINT('Ctrl Pts',(5.98145286361836,-20.9850401822713,21.));
#9621=CARTESIAN_POINT('Ctrl Pts',(6.01930117633044,-21.0208530236003,0.));
#9622=CARTESIAN_POINT('Ctrl Pts',(6.01930117633044,-21.0208530236003,21.));
#9623=CARTESIAN_POINT('Ctrl Pts',(6.05737013696532,-21.0565393163693,0.));
#9624=CARTESIAN_POINT('Ctrl Pts',(6.05737013696532,-21.0565393163693,21.));
#9625=CARTESIAN_POINT('Ctrl Pts',(6.08800133883114,-21.0849872356853,0.));
#9626=CARTESIAN_POINT('Ctrl Pts',(6.08800133883114,-21.0849872356853,21.));
#9627=CARTESIAN_POINT('Ctrl Pts',(6.11107360216957,-21.1062663590356,0.));
#9628=CARTESIAN_POINT('Ctrl Pts',(6.11107360216957,-21.1062663590356,21.));
#9629=CARTESIAN_POINT('Ctrl Pts',(6.12649903511517,-21.1204271980506,0.));
#9630=CARTESIAN_POINT('Ctrl Pts',(6.12649903511517,-21.1204271980506,21.));
#9631=CARTESIAN_POINT('Ctrl Pts',(6.1342227326009,-21.1275013067528,0.));
#9632=CARTESIAN_POINT('Ctrl Pts',(6.1342227326009,-21.1275013067528,21.));
#9633=CARTESIAN_POINT('Ctrl Pts',(4.1144891981253,-18.337935196262,0.));
#9634=CARTESIAN_POINT('Ctrl Pts',(4.11655269114951,-18.3471320125699,0.));
#9635=CARTESIAN_POINT('Ctrl Pts',(4.12092019868859,-18.3654573320481,0.));
#9636=CARTESIAN_POINT('Ctrl Pts',(4.12819301671078,-18.3927403741815,0.));
#9637=CARTESIAN_POINT('Ctrl Pts',(4.13926275457062,-18.4287286547442,0.));
#9638=CARTESIAN_POINT('Ctrl Pts',(4.15497867673974,-18.4731856794913,0.));
#9639=CARTESIAN_POINT('Ctrl Pts',(4.17205262766561,-18.5172668097744,0.));
#9640=CARTESIAN_POINT('Ctrl Pts',(4.1899696727862,-18.5611217636409,0.));
#9641=CARTESIAN_POINT('Ctrl Pts',(4.20834600700664,-18.6048602364653,0.));
#9642=CARTESIAN_POINT('Ctrl Pts',(4.22703266508918,-18.6485210883348,0.));
#9643=CARTESIAN_POINT('Ctrl Pts',(4.24603817988452,-18.6920958920047,0.));
#9644=CARTESIAN_POINT('Ctrl Pts',(4.26546636161932,-18.735547949685,0.));
#9645=CARTESIAN_POINT('Ctrl Pts',(4.28545098663152,-18.778832216358,0.));
#9646=CARTESIAN_POINT('Ctrl Pts',(4.30608591031525,-18.8219166495975,0.));
#9647=CARTESIAN_POINT('Ctrl Pts',(4.32737526247704,-18.8647973781745,0.));
#9648=CARTESIAN_POINT('Ctrl Pts',(4.34926881342021,-18.9074876952706,0.));
#9649=CARTESIAN_POINT('Ctrl Pts',(4.37168516143122,-18.9500107909187,0.));
#9650=CARTESIAN_POINT('Ctrl Pts',(4.39453820875554,-18.9923914823906,0.));
#9651=CARTESIAN_POINT('Ctrl Pts',(4.41776558033331,-19.034647328575,0.));
#9652=CARTESIAN_POINT('Ctrl Pts',(4.44134542994081,-19.0767833717249,0.));
#9653=CARTESIAN_POINT('Ctrl Pts',(4.46528051067021,-19.1187970904933,0.));
#9654=CARTESIAN_POINT('Ctrl Pts',(4.48958819710576,-19.1606814968494,0.));
#9655=CARTESIAN_POINT('Ctrl Pts',(4.51428889122954,-19.2024287376926,0.));
#9656=CARTESIAN_POINT('Ctrl Pts',(4.53939338835151,-19.2440340196551,0.));
#9657=CARTESIAN_POINT('Ctrl Pts',(4.5648965160674,-19.2854975819105,0.));
#9658=CARTESIAN_POINT('Ctrl Pts',(4.59078395765677,-19.3268225655679,0.));
#9659=CARTESIAN_POINT('Ctrl Pts',(4.61703633725711,-19.3680137353983,0.));
#9660=CARTESIAN_POINT('Ctrl Pts',(4.64363405547472,-19.4090759683639,0.));
#9661=CARTESIAN_POINT('Ctrl Pts',(4.67056260851452,-19.4500125912299,0.));
#9662=CARTESIAN_POINT('Ctrl Pts',(4.69781487613784,-19.4908246636763,0.));
#9663=CARTESIAN_POINT('Ctrl Pts',(4.72538815796615,-19.531511899192,0.));
#9664=CARTESIAN_POINT('Ctrl Pts',(4.7532823819461,-19.5720732205813,0.));
#9665=CARTESIAN_POINT('Ctrl Pts',(4.7814979936173,-19.6125074152527,0.));
#9666=CARTESIAN_POINT('Ctrl Pts',(4.8100336141806,-19.6528138625329,0.));
#9667=CARTESIAN_POINT('Ctrl Pts',(4.83888510708974,-19.6929928227072,0.));
#9668=CARTESIAN_POINT('Ctrl Pts',(4.86804682289086,-19.7330450480715,0.));
#9669=CARTESIAN_POINT('Ctrl Pts',(4.89751233527804,-19.772971552601,0.));
#9670=CARTESIAN_POINT('Ctrl Pts',(4.92727531494346,-19.8127733387903,0.));
#9671=CARTESIAN_POINT('Ctrl Pts',(4.95733049830095,-19.8524510953961,0.));
#9672=CARTESIAN_POINT('Ctrl Pts',(4.98767405031333,-19.8920050831202,0.));
#9673=CARTESIAN_POINT('Ctrl Pts',(5.01830302225557,-19.931435301086,0.));
#9674=CARTESIAN_POINT('Ctrl Pts',(5.04921502064063,-19.9707415879783,0.));
#9675=CARTESIAN_POINT('Ctrl Pts',(5.08040781745336,-20.0099237417205,0.));
#9676=CARTESIAN_POINT('Ctrl Pts',(5.11187891582334,-20.0489816528155,0.));
#9677=CARTESIAN_POINT('Ctrl Pts',(5.14362537555397,-20.087915358486,0.));
#9678=CARTESIAN_POINT('Ctrl Pts',(5.17564404279921,-20.1267249732337,0.));
#9679=CARTESIAN_POINT('Ctrl Pts',(5.20793168386163,-20.1654106491899,0.));
#9680=CARTESIAN_POINT('Ctrl Pts',(5.2404851444189,-20.2039725283917,0.));
#9681=CARTESIAN_POINT('Ctrl Pts',(5.27330152298149,-20.2424106921768,0.));
#9682=CARTESIAN_POINT('Ctrl Pts',(5.30637824220997,-20.2807251380077,0.));
#9683=CARTESIAN_POINT('Ctrl Pts',(5.33971294212213,-20.3189158047642,0.));
#9684=CARTESIAN_POINT('Ctrl Pts',(5.37330341114648,-20.3569825877537,0.));
#9685=CARTESIAN_POINT('Ctrl Pts',(5.40714750595874,-20.3949253578015,0.));
#9686=CARTESIAN_POINT('Ctrl Pts',(5.4412430606511,-20.4327439816542,0.));
#9687=CARTESIAN_POINT('Ctrl Pts',(5.4755878444985,-20.4704383353718,0.));
#9688=CARTESIAN_POINT('Ctrl Pts',(5.51017962306782,-20.5080083009242,0.));
#9689=CARTESIAN_POINT('Ctrl Pts',(5.54501619689459,-20.5454537676144,0.));
#9690=CARTESIAN_POINT('Ctrl Pts',(5.58009544402474,-20.5827746317185,0.));
#9691=CARTESIAN_POINT('Ctrl Pts',(5.61541536715148,-20.6199707996366,0.));
#9692=CARTESIAN_POINT('Ctrl Pts',(5.65097411164334,-20.6570421847033,0.));
#9693=CARTESIAN_POINT('Ctrl Pts',(5.68676990500163,-20.6939886877061,0.));
#9694=CARTESIAN_POINT('Ctrl Pts',(5.7228010079824,-20.7308101804425,0.));
#9695=CARTESIAN_POINT('Ctrl Pts',(5.75906566327795,-20.7675064905026,0.));
#9696=CARTESIAN_POINT('Ctrl Pts',(5.79556203439643,-20.8040773827343,0.));
#9697=CARTESIAN_POINT('Ctrl Pts',(5.83228817460177,-20.8405225541277,0.));
#9698=CARTESIAN_POINT('Ctrl Pts',(5.86924212736287,-20.8768416821402,0.));
#9699=CARTESIAN_POINT('Ctrl Pts',(5.90642200662599,-20.9130344665641,0.));
#9700=CARTESIAN_POINT('Ctrl Pts',(5.94382608200804,-20.9491006734021,0.));
#9701=CARTESIAN_POINT('Ctrl Pts',(5.98145286361836,-20.9850401822713,0.));
#9702=CARTESIAN_POINT('Ctrl Pts',(6.02687083887286,-21.0280155918661,0.));
#9703=CARTESIAN_POINT('Ctrl Pts',(6.06499496148844,-21.0636702474951,0.));
#9704=CARTESIAN_POINT('Ctrl Pts',(6.09567013127871,-21.0920928984154,0.));
#9705=CARTESIAN_POINT('Ctrl Pts',(6.118775337615,-21.1133530893457,0.));
#9706=CARTESIAN_POINT('Ctrl Pts',(6.1342227326009,-21.1275013067528,0.));
#9707=CARTESIAN_POINT('Ctrl Pts',(4.1144891981253,-18.337935196262,13.));
#9708=CARTESIAN_POINT('Ctrl Pts',(4.11796712887951,-18.3534360435645,13.));
#9709=CARTESIAN_POINT('Ctrl Pts',(4.12185943358937,-18.3688191548995,13.));
#9710=CARTESIAN_POINT('Ctrl Pts',(4.12613856044267,-18.3840926404824,13.));
#9711=CARTESIAN_POINT('Ctrl Pts',(4.13115401716692,-18.4019943079477,13.));
#9712=CARTESIAN_POINT('Ctrl Pts',(4.13670006307401,-18.4197456248295,13.));
#9713=CARTESIAN_POINT('Ctrl Pts',(4.1426637807957,-18.4373797424196,13.));
#9714=CARTESIAN_POINT('Ctrl Pts',(4.15105501703309,-18.4621917897769,13.));
#9715=CARTESIAN_POINT('Ctrl Pts',(4.16026629328986,-18.4867739015683,13.));
#9716=CARTESIAN_POINT('Ctrl Pts',(4.16990400115282,-18.5112408492934,13.));
#9717=CARTESIAN_POINT('Ctrl Pts',(4.17631459686346,-18.5275152282609,13.));
#9718=CARTESIAN_POINT('Ctrl Pts',(4.18291190640786,-18.5437392096496,13.));
#9719=CARTESIAN_POINT('Ctrl Pts',(4.18960898617043,-18.5599376581358,13.));
#9720=CARTESIAN_POINT('Ctrl Pts',(4.19665876042785,-18.5769891804704,13.));
#9721=CARTESIAN_POINT('Ctrl Pts',(4.20381824254442,-18.5940126577989,13.));
#9722=CARTESIAN_POINT('Ctrl Pts',(4.21104759333806,-18.6110185062838,13.));
#9723=CARTESIAN_POINT('Ctrl Pts',(4.21907618313383,-18.6299044319376,13.));
#9724=CARTESIAN_POINT('Ctrl Pts',(4.22719219297436,-18.6487682283615,13.));
#9725=CARTESIAN_POINT('Ctrl Pts',(4.23540730606873,-18.6676042988365,13.));
#9726=CARTESIAN_POINT('Ctrl Pts',(4.24779198778708,-18.6960005893047,13.));
#9727=CARTESIAN_POINT('Ctrl Pts',(4.26040793123128,-18.7243319351566,13.));
#9728=CARTESIAN_POINT('Ctrl Pts',(4.27340283281643,-18.7525479285623,13.));
#9729=CARTESIAN_POINT('Ctrl Pts',(4.28284334471928,-18.7730462309044,13.));
#9730=CARTESIAN_POINT('Ctrl Pts',(4.29248702330027,-18.7934827312566,13.));
#9731=CARTESIAN_POINT('Ctrl Pts',(4.302353207313,-18.8138501272208,13.));
#9732=CARTESIAN_POINT('Ctrl Pts',(4.31441377244323,-18.8387475247599,13.));
#9733=CARTESIAN_POINT('Ctrl Pts',(4.32680560862706,-18.8635420328946,13.));
#9734=CARTESIAN_POINT('Ctrl Pts',(4.33948253068719,-18.8882460103694,13.));
#9735=CARTESIAN_POINT('Ctrl Pts',(4.35317571045417,-18.9149304060703,13.));
#9736=CARTESIAN_POINT('Ctrl Pts',(4.36719580768616,-18.9415109549169,13.));
#9737=CARTESIAN_POINT('Ctrl Pts',(4.38145466528598,-18.9680129070804,13.));
#9738=CARTESIAN_POINT('Ctrl Pts',(4.39461837564025,-18.9924793848231,13.));
#9739=CARTESIAN_POINT('Ctrl Pts',(4.40798318219245,-19.0168796293508,13.));
#9740=CARTESIAN_POINT('Ctrl Pts',(4.42152146523896,-19.0412206988271,13.));
#9741=CARTESIAN_POINT('Ctrl Pts',(4.43991391790099,-19.0742892915392,13.));
#9742=CARTESIAN_POINT('Ctrl Pts',(4.45862842583093,-19.1072480695959,13.));
#9743=CARTESIAN_POINT('Ctrl Pts',(4.47769255669439,-19.1400849917414,13.));
#9744=CARTESIAN_POINT('Ctrl Pts',(4.49608903122715,-19.1717719123942,13.));
#9745=CARTESIAN_POINT('Ctrl Pts',(4.51481852753143,-19.2033430485072,13.));
#9746=CARTESIAN_POINT('Ctrl Pts',(4.53389559693718,-19.2347910924796,13.));
#9747=CARTESIAN_POINT('Ctrl Pts',(4.55981233024546,-19.2775141413591,13.));
#9748=CARTESIAN_POINT('Ctrl Pts',(4.58636743987533,-19.3200109593949,13.));
#9749=CARTESIAN_POINT('Ctrl Pts',(4.61347737187984,-19.362301314555,13.));
#9750=CARTESIAN_POINT('Ctrl Pts',(4.63730641274119,-19.3994736173474,13.));
#9751=CARTESIAN_POINT('Ctrl Pts',(4.66155758397822,-19.4364884575386,13.));
#9752=CARTESIAN_POINT('Ctrl Pts',(4.68619912960012,-19.4733518508001,13.));
#9753=CARTESIAN_POINT('Ctrl Pts',(4.72252675031123,-19.527697442147,13.));
#9754=CARTESIAN_POINT('Ctrl Pts',(4.7597114391618,-19.5817111528721,13.));
#9755=CARTESIAN_POINT('Ctrl Pts',(4.79774570305514,-19.6353839065428,13.));
#9756=CARTESIAN_POINT('Ctrl Pts',(4.84574531526665,-19.7031194454701,13.));
#9757=CARTESIAN_POINT('Ctrl Pts',(4.89509304274286,-19.7703134648063,13.));
#9758=CARTESIAN_POINT('Ctrl Pts',(4.94566457622742,-19.8369838018677,13.));
#9759=CARTESIAN_POINT('Ctrl Pts',(5.01416761732255,-19.9272939136015,13.));
#9760=CARTESIAN_POINT('Ctrl Pts',(5.08492180316416,-20.0166413603291,13.));
#9761=CARTESIAN_POINT('Ctrl Pts',(5.15778644842965,-20.1050225704803,13.));
#9762=CARTESIAN_POINT('Ctrl Pts',(5.22274718796653,-20.1838167339825,13.));
#9763=CARTESIAN_POINT('Ctrl Pts',(5.28937724256698,-20.2618454270028,13.));
#9764=CARTESIAN_POINT('Ctrl Pts',(5.35757729677352,-20.3391090335982,13.));
#9765=CARTESIAN_POINT('Ctrl Pts',(5.45423552752918,-20.4486128104235,13.));
#9766=CARTESIAN_POINT('Ctrl Pts',(5.55405240994679,-20.5565772403027,13.));
#9767=CARTESIAN_POINT('Ctrl Pts',(5.65680258312696,-20.662990693601,13.));
#9768=CARTESIAN_POINT('Ctrl Pts',(5.73661648094275,-20.7456501405381,13.));
#9769=CARTESIAN_POINT('Ctrl Pts',(5.81820510837542,-20.8273750321949,13.));
#9770=CARTESIAN_POINT('Ctrl Pts',(5.90147459238375,-20.9081522149626,13.));
#9771=CARTESIAN_POINT('Ctrl Pts',(5.97350899070235,-20.9780305843057,13.));
#9772=CARTESIAN_POINT('Ctrl Pts',(6.04679718623577,-21.0471984384854,13.));
#9773=CARTESIAN_POINT('Ctrl Pts',(6.12131239423385,-21.1156584428611,13.));
#9774=CARTESIAN_POINT('Ctrl Pts',(6.12561174166735,-21.1196084196781,13.));
#9775=CARTESIAN_POINT('Ctrl Pts',(6.12991518786664,-21.1235560409334,13.));
#9776=CARTESIAN_POINT('Ctrl Pts',(6.1342227326009,-21.1275013067528,13.));
#9777=CARTESIAN_POINT('Ctrl Pts',(0.694764450219577,-21.9890268624765,0.));
#9778=CARTESIAN_POINT('Ctrl Pts',(0.694764450219577,-21.9890268624765,21.));
#9779=CARTESIAN_POINT('Ctrl Pts',(0.699924103234218,-21.9799122315157,0.));
#9780=CARTESIAN_POINT('Ctrl Pts',(0.699924103234218,-21.9799122315157,21.));
#9781=CARTESIAN_POINT('Ctrl Pts',(0.710218621843551,-21.9616777523685,0.));
#9782=CARTESIAN_POINT('Ctrl Pts',(0.710218621843551,-21.9616777523685,21.));
#9783=CARTESIAN_POINT('Ctrl Pts',(0.725586037496632,-21.9343103819749,0.));
#9784=CARTESIAN_POINT('Ctrl Pts',(0.725586037496632,-21.9343103819749,21.));
#9785=CARTESIAN_POINT('Ctrl Pts',(0.745927151109818,-21.8977892409997,0.));
#9786=CARTESIAN_POINT('Ctrl Pts',(0.745927151109818,-21.8977892409997,21.));
#9787=CARTESIAN_POINT('Ctrl Pts',(0.771105213258327,-21.8520856039249,0.));
#9788=CARTESIAN_POINT('Ctrl Pts',(0.771105213258327,-21.8520856039249,21.));
#9789=CARTESIAN_POINT('Ctrl Pts',(0.796034321106407,-21.8063297959755,0.));
#9790=CARTESIAN_POINT('Ctrl Pts',(0.796034321106407,-21.8063297959755,21.));
#9791=CARTESIAN_POINT('Ctrl Pts',(0.820713597934075,-21.7605219769118,0.));
#9792=CARTESIAN_POINT('Ctrl Pts',(0.820713597934075,-21.7605219769118,21.));
#9793=CARTESIAN_POINT('Ctrl Pts',(0.845141916726555,-21.7146624809285,0.));
#9794=CARTESIAN_POINT('Ctrl Pts',(0.845141916726555,-21.7146624809285,21.));
#9795=CARTESIAN_POINT('Ctrl Pts',(0.869317897714094,-21.6687518829182,0.));
#9796=CARTESIAN_POINT('Ctrl Pts',(0.869317897714094,-21.6687518829182,21.));
#9797=CARTESIAN_POINT('Ctrl Pts',(0.89323996751367,-21.6227909401433,0.));
#9798=CARTESIAN_POINT('Ctrl Pts',(0.89323996751367,-21.6227909401433,21.));
#9799=CARTESIAN_POINT('Ctrl Pts',(0.916906425150851,-21.5767805209408,0.));
#9800=CARTESIAN_POINT('Ctrl Pts',(0.916906425150851,-21.5767805209408,21.));
#9801=CARTESIAN_POINT('Ctrl Pts',(0.940315509525146,-21.5307215366685,0.));
#9802=CARTESIAN_POINT('Ctrl Pts',(0.940315509525146,-21.5307215366685,21.));
#9803=CARTESIAN_POINT('Ctrl Pts',(0.963465462815768,-21.4846148770804,0.));
#9804=CARTESIAN_POINT('Ctrl Pts',(0.963465462815768,-21.4846148770804,21.));
#9805=CARTESIAN_POINT('Ctrl Pts',(0.986354611081129,-21.4384613333266,0.));
#9806=CARTESIAN_POINT('Ctrl Pts',(0.986354611081129,-21.4384613333266,21.));
#9807=CARTESIAN_POINT('Ctrl Pts',(1.00898133629987,-21.3922616124166,0.));
#9808=CARTESIAN_POINT('Ctrl Pts',(1.00898133629987,-21.3922616124166,21.));
#9809=CARTESIAN_POINT('Ctrl Pts',(1.03134402396952,-21.3460163737343,0.));
#9810=CARTESIAN_POINT('Ctrl Pts',(1.03134402396952,-21.3460163737343,21.));
#9811=CARTESIAN_POINT('Ctrl Pts',(1.05344101900192,-21.2997262593683,0.));
#9812=CARTESIAN_POINT('Ctrl Pts',(1.05344101900192,-21.2997262593683,21.));
#9813=CARTESIAN_POINT('Ctrl Pts',(1.07527058431887,-21.2533919248553,0.));
#9814=CARTESIAN_POINT('Ctrl Pts',(1.07527058431887,-21.2533919248553,21.));
#9815=CARTESIAN_POINT('Ctrl Pts',(1.09683084929265,-21.2070140764156,0.));
#9816=CARTESIAN_POINT('Ctrl Pts',(1.09683084929265,-21.2070140764156,21.));
#9817=CARTESIAN_POINT('Ctrl Pts',(1.11811982787746,-21.1605934684164,0.));
#9818=CARTESIAN_POINT('Ctrl Pts',(1.11811982787746,-21.1605934684164,21.));
#9819=CARTESIAN_POINT('Ctrl Pts',(1.13913546246554,-21.1141308858087,0.));
#9820=CARTESIAN_POINT('Ctrl Pts',(1.13913546246554,-21.1141308858087,21.));
#9821=CARTESIAN_POINT('Ctrl Pts',(1.15987566445807,-21.0676271313238,0.));
#9822=CARTESIAN_POINT('Ctrl Pts',(1.15987566445807,-21.0676271313238,21.));
#9823=CARTESIAN_POINT('Ctrl Pts',(1.18033835060894,-21.0210830121673,0.));
#9824=CARTESIAN_POINT('Ctrl Pts',(1.18033835060894,-21.0210830121673,21.));
#9825=CARTESIAN_POINT('Ctrl Pts',(1.20052150219502,-20.9744993243732,0.));
#9826=CARTESIAN_POINT('Ctrl Pts',(1.20052150219502,-20.9744993243732,21.));
#9827=CARTESIAN_POINT('Ctrl Pts',(1.22042312071096,-20.9278768531175,0.));
#9828=CARTESIAN_POINT('Ctrl Pts',(1.22042312071096,-20.9278768531175,21.));
#9829=CARTESIAN_POINT('Ctrl Pts',(1.24004113517905,-20.881216381382,0.));
#9830=CARTESIAN_POINT('Ctrl Pts',(1.24004113517905,-20.881216381382,21.));
#9831=CARTESIAN_POINT('Ctrl Pts',(1.25937332001004,-20.83451869657,0.));
#9832=CARTESIAN_POINT('Ctrl Pts',(1.25937332001004,-20.83451869657,21.));
#9833=CARTESIAN_POINT('Ctrl Pts',(1.27841722479261,-20.7877845975367,0.));
#9834=CARTESIAN_POINT('Ctrl Pts',(1.27841722479261,-20.7877845975367,21.));
#9835=CARTESIAN_POINT('Ctrl Pts',(1.29717006491149,-20.7410149035348,0.));
#9836=CARTESIAN_POINT('Ctrl Pts',(1.29717006491149,-20.7410149035348,21.));
#9837=CARTESIAN_POINT('Ctrl Pts',(1.31562879653596,-20.694210454218,0.));
#9838=CARTESIAN_POINT('Ctrl Pts',(1.31562879653596,-20.694210454218,21.));
#9839=CARTESIAN_POINT('Ctrl Pts',(1.3337902972259,-20.6473721041685,0.));
#9840=CARTESIAN_POINT('Ctrl Pts',(1.3337902972259,-20.6473721041685,21.));
#9841=CARTESIAN_POINT('Ctrl Pts',(1.35165153211252,-20.6005007190809,0.));
#9842=CARTESIAN_POINT('Ctrl Pts',(1.35165153211252,-20.6005007190809,21.));
#9843=CARTESIAN_POINT('Ctrl Pts',(1.36920969340018,-20.5535971721246,0.));
#9844=CARTESIAN_POINT('Ctrl Pts',(1.36920969340018,-20.5535971721246,21.));
#9845=CARTESIAN_POINT('Ctrl Pts',(1.38646244026049,-20.5066623390132,0.));
#9846=CARTESIAN_POINT('Ctrl Pts',(1.38646244026049,-20.5066623390132,21.));
#9847=CARTESIAN_POINT('Ctrl Pts',(1.40340771617024,-20.4596971004275,0.));
#9848=CARTESIAN_POINT('Ctrl Pts',(1.40340771617024,-20.4596971004275,21.));
#9849=CARTESIAN_POINT('Ctrl Pts',(1.42004329463709,-20.4127023494155,0.));
#9850=CARTESIAN_POINT('Ctrl Pts',(1.42004329463709,-20.4127023494155,21.));
#9851=CARTESIAN_POINT('Ctrl Pts',(1.43636637152782,-20.3656789980171,0.));
#9852=CARTESIAN_POINT('Ctrl Pts',(1.43636637152782,-20.3656789980171,21.));
#9853=CARTESIAN_POINT('Ctrl Pts',(1.45237321894403,-20.3186279833818,0.));
#9854=CARTESIAN_POINT('Ctrl Pts',(1.45237321894403,-20.3186279833818,21.));
#9855=CARTESIAN_POINT('Ctrl Pts',(1.4680586180802,-20.2715502770004,0.));
#9856=CARTESIAN_POINT('Ctrl Pts',(1.4680586180802,-20.2715502770004,21.));
#9857=CARTESIAN_POINT('Ctrl Pts',(1.48341623961913,-20.224446881308,0.));
#9858=CARTESIAN_POINT('Ctrl Pts',(1.48341623961913,-20.224446881308,21.));
#9859=CARTESIAN_POINT('Ctrl Pts',(1.49843965844501,-20.1773188177942,0.));
#9860=CARTESIAN_POINT('Ctrl Pts',(1.49843965844501,-20.1773188177942,21.));
#9861=CARTESIAN_POINT('Ctrl Pts',(1.51312326913582,-20.1301671167606,0.));
#9862=CARTESIAN_POINT('Ctrl Pts',(1.51312326913582,-20.1301671167606,21.));
#9863=CARTESIAN_POINT('Ctrl Pts',(1.52746305716964,-20.0829928089241,0.));
#9864=CARTESIAN_POINT('Ctrl Pts',(1.52746305716964,-20.0829928089241,21.));
#9865=CARTESIAN_POINT('Ctrl Pts',(1.54145790302917,-20.0357969106526,0.));
#9866=CARTESIAN_POINT('Ctrl Pts',(1.54145790302917,-20.0357969106526,21.));
#9867=CARTESIAN_POINT('Ctrl Pts',(1.55510860515913,-19.9885804375097,0.));
#9868=CARTESIAN_POINT('Ctrl Pts',(1.55510860515913,-19.9885804375097,21.));
#9869=CARTESIAN_POINT('Ctrl Pts',(1.56841542790452,-19.9413444362352,0.));
#9870=CARTESIAN_POINT('Ctrl Pts',(1.56841542790452,-19.9413444362352,21.));
#9871=CARTESIAN_POINT('Ctrl Pts',(1.58137589158952,-19.8940900137801,0.));
#9872=CARTESIAN_POINT('Ctrl Pts',(1.58137589158952,-19.8940900137801,21.));
#9873=CARTESIAN_POINT('Ctrl Pts',(1.59398289700558,-19.8468183626037,0.));
#9874=CARTESIAN_POINT('Ctrl Pts',(1.59398289700558,-19.8468183626037,21.));
#9875=CARTESIAN_POINT('Ctrl Pts',(1.60622162219699,-19.7995308006834,0.));
#9876=CARTESIAN_POINT('Ctrl Pts',(1.60622162219699,-19.7995308006834,21.));
#9877=CARTESIAN_POINT('Ctrl Pts',(1.61807191996833,-19.7522287462982,0.));
#9878=CARTESIAN_POINT('Ctrl Pts',(1.61807191996833,-19.7522287462982,21.));
#9879=CARTESIAN_POINT('Ctrl Pts',(1.62951389038421,-19.7049136553525,0.));
#9880=CARTESIAN_POINT('Ctrl Pts',(1.62951389038421,-19.7049136553525,21.));
#9881=CARTESIAN_POINT('Ctrl Pts',(1.64053294677821,-19.6575869645839,0.));
#9882=CARTESIAN_POINT('Ctrl Pts',(1.64053294677821,-19.6575869645839,21.));
#9883=CARTESIAN_POINT('Ctrl Pts',(1.65112409599282,-19.6102500448855,0.));
#9884=CARTESIAN_POINT('Ctrl Pts',(1.65112409599282,-19.6102500448855,21.));
#9885=CARTESIAN_POINT('Ctrl Pts',(1.66129908621006,-19.5629041190868,0.));
#9886=CARTESIAN_POINT('Ctrl Pts',(1.66129908621006,-19.5629041190868,21.));
#9887=CARTESIAN_POINT('Ctrl Pts',(1.67107974760948,-19.5155503513712,0.));
#9888=CARTESIAN_POINT('Ctrl Pts',(1.67107974760948,-19.5155503513712,21.));
#9889=CARTESIAN_POINT('Ctrl Pts',(1.68048476382294,-19.4681900187091,0.));
#9890=CARTESIAN_POINT('Ctrl Pts',(1.68048476382294,-19.4681900187091,21.));
#9891=CARTESIAN_POINT('Ctrl Pts',(1.6895175323357,-19.4208246682917,0.));
#9892=CARTESIAN_POINT('Ctrl Pts',(1.6895175323357,-19.4208246682917,21.));
#9893=CARTESIAN_POINT('Ctrl Pts',(1.69815571801251,-19.3734562555057,0.));
#9894=CARTESIAN_POINT('Ctrl Pts',(1.69815571801251,-19.3734562555057,21.));
#9895=CARTESIAN_POINT('Ctrl Pts',(1.70633457265124,-19.3260873558094,0.));
#9896=CARTESIAN_POINT('Ctrl Pts',(1.70633457265124,-19.3260873558094,21.));
#9897=CARTESIAN_POINT('Ctrl Pts',(1.71396454346262,-19.2787209722437,0.));
#9898=CARTESIAN_POINT('Ctrl Pts',(1.71396454346262,-19.2787209722437,21.));
#9899=CARTESIAN_POINT('Ctrl Pts',(1.72096104670233,-19.2313602042899,0.));
#9900=CARTESIAN_POINT('Ctrl Pts',(1.72096104670233,-19.2313602042899,21.));
#9901=CARTESIAN_POINT('Ctrl Pts',(1.72727220327097,-19.1840079312107,0.));
#9902=CARTESIAN_POINT('Ctrl Pts',(1.72727220327097,-19.1840079312107,21.));
#9903=CARTESIAN_POINT('Ctrl Pts',(1.73290313712353,-19.1366665585833,0.));
#9904=CARTESIAN_POINT('Ctrl Pts',(1.73290313712353,-19.1366665585833,21.));
#9905=CARTESIAN_POINT('Ctrl Pts',(1.7379530116984,-19.0893375576541,0.));
#9906=CARTESIAN_POINT('Ctrl Pts',(1.7379530116984,-19.0893375576541,21.));
#9907=CARTESIAN_POINT('Ctrl Pts',(1.74256297552948,-19.0420224296189,0.));
#9908=CARTESIAN_POINT('Ctrl Pts',(1.74256297552948,-19.0420224296189,21.));
#9909=CARTESIAN_POINT('Ctrl Pts',(1.74684309825012,-18.9947239970259,0.));
#9910=CARTESIAN_POINT('Ctrl Pts',(1.74684309825012,-18.9947239970259,21.));
#9911=CARTESIAN_POINT('Ctrl Pts',(1.75080409924533,-18.947447637865,0.));
#9912=CARTESIAN_POINT('Ctrl Pts',(1.75080409924533,-18.947447637865,21.));
#9913=CARTESIAN_POINT('Ctrl Pts',(1.75429229572775,-18.9002024267872,0.));
#9914=CARTESIAN_POINT('Ctrl Pts',(1.75429229572775,-18.9002024267872,21.));
#9915=CARTESIAN_POINT('Ctrl Pts',(1.75690876962597,-18.8530026395886,0.));
#9916=CARTESIAN_POINT('Ctrl Pts',(1.75690876962597,-18.8530026395886,21.));
#9917=CARTESIAN_POINT('Ctrl Pts',(1.7581175236483,-18.8058650094753,0.));
#9918=CARTESIAN_POINT('Ctrl Pts',(1.7581175236483,-18.8058650094753,21.));
#9919=CARTESIAN_POINT('Ctrl Pts',(1.75752447968136,-18.7682173836138,0.));
#9920=CARTESIAN_POINT('Ctrl Pts',(1.75752447968136,-18.7682173836138,21.));
#9921=CARTESIAN_POINT('Ctrl Pts',(1.75601041697575,-18.7400222442427,0.));
#9922=CARTESIAN_POINT('Ctrl Pts',(1.75601041697575,-18.7400222442427,21.));
#9923=CARTESIAN_POINT('Ctrl Pts',(1.75450132833463,-18.7212441956871,0.));
#9924=CARTESIAN_POINT('Ctrl Pts',(1.75450132833463,-18.7212441956871,21.));
#9925=CARTESIAN_POINT('Ctrl Pts',(1.75362185428836,-18.7118598491961,0.));
#9926=CARTESIAN_POINT('Ctrl Pts',(1.75362185428836,-18.7118598491961,21.));
#9927=CARTESIAN_POINT('',(0.69476445021964,-21.9890268624765,0.));
#9928=CARTESIAN_POINT('Ctrl Pts',(1.75362185428836,-18.7118598491961,0.));
#9929=CARTESIAN_POINT('Ctrl Pts',(1.75450132833463,-18.7212441956871,0.));
#9930=CARTESIAN_POINT('Ctrl Pts',(1.75601041697575,-18.7400222442427,0.));
#9931=CARTESIAN_POINT('Ctrl Pts',(1.75752447968136,-18.7682173836138,0.));
#9932=CARTESIAN_POINT('Ctrl Pts',(1.7581175236483,-18.8058650094753,0.));
#9933=CARTESIAN_POINT('Ctrl Pts',(1.75690876962597,-18.8530026395886,0.));
#9934=CARTESIAN_POINT('Ctrl Pts',(1.75429229572775,-18.9002024267872,0.));
#9935=CARTESIAN_POINT('Ctrl Pts',(1.75080409924533,-18.947447637865,0.));
#9936=CARTESIAN_POINT('Ctrl Pts',(1.74684309825012,-18.9947239970259,0.));
#9937=CARTESIAN_POINT('Ctrl Pts',(1.74256297552948,-19.0420224296189,0.));
#9938=CARTESIAN_POINT('Ctrl Pts',(1.7379530116984,-19.0893375576541,0.));
#9939=CARTESIAN_POINT('Ctrl Pts',(1.73290313712353,-19.1366665585833,0.));
#9940=CARTESIAN_POINT('Ctrl Pts',(1.72727220327097,-19.1840079312107,0.));
#9941=CARTESIAN_POINT('Ctrl Pts',(1.72096104670233,-19.2313602042899,0.));
#9942=CARTESIAN_POINT('Ctrl Pts',(1.71396454346262,-19.2787209722437,0.));
#9943=CARTESIAN_POINT('Ctrl Pts',(1.70633457265124,-19.3260873558094,0.));
#9944=CARTESIAN_POINT('Ctrl Pts',(1.69815571801251,-19.3734562555057,0.));
#9945=CARTESIAN_POINT('Ctrl Pts',(1.6895175323357,-19.4208246682917,0.));
#9946=CARTESIAN_POINT('Ctrl Pts',(1.68048476382294,-19.4681900187091,0.));
#9947=CARTESIAN_POINT('Ctrl Pts',(1.67107974760948,-19.5155503513712,0.));
#9948=CARTESIAN_POINT('Ctrl Pts',(1.66129908621006,-19.5629041190868,0.));
#9949=CARTESIAN_POINT('Ctrl Pts',(1.65112409599282,-19.6102500448855,0.));
#9950=CARTESIAN_POINT('Ctrl Pts',(1.64053294677821,-19.6575869645839,0.));
#9951=CARTESIAN_POINT('Ctrl Pts',(1.62951389038421,-19.7049136553525,0.));
#9952=CARTESIAN_POINT('Ctrl Pts',(1.61807191996833,-19.7522287462982,0.));
#9953=CARTESIAN_POINT('Ctrl Pts',(1.60622162219699,-19.7995308006834,0.));
#9954=CARTESIAN_POINT('Ctrl Pts',(1.59398289700558,-19.8468183626037,0.));
#9955=CARTESIAN_POINT('Ctrl Pts',(1.58137589158952,-19.8940900137801,0.));
#9956=CARTESIAN_POINT('Ctrl Pts',(1.56841542790452,-19.9413444362352,0.));
#9957=CARTESIAN_POINT('Ctrl Pts',(1.55510860515913,-19.9885804375097,0.));
#9958=CARTESIAN_POINT('Ctrl Pts',(1.54145790302917,-20.0357969106526,0.));
#9959=CARTESIAN_POINT('Ctrl Pts',(1.52746305716964,-20.0829928089241,0.));
#9960=CARTESIAN_POINT('Ctrl Pts',(1.51312326913582,-20.1301671167606,0.));
#9961=CARTESIAN_POINT('Ctrl Pts',(1.49843965844501,-20.1773188177942,0.));
#9962=CARTESIAN_POINT('Ctrl Pts',(1.48341623961913,-20.224446881308,0.));
#9963=CARTESIAN_POINT('Ctrl Pts',(1.4680586180802,-20.2715502770004,0.));
#9964=CARTESIAN_POINT('Ctrl Pts',(1.45237321894403,-20.3186279833818,0.));
#9965=CARTESIAN_POINT('Ctrl Pts',(1.43636637152782,-20.3656789980171,0.));
#9966=CARTESIAN_POINT('Ctrl Pts',(1.42004329463709,-20.4127023494155,0.));
#9967=CARTESIAN_POINT('Ctrl Pts',(1.40340771617024,-20.4596971004275,0.));
#9968=CARTESIAN_POINT('Ctrl Pts',(1.38646244026049,-20.5066623390132,0.));
#9969=CARTESIAN_POINT('Ctrl Pts',(1.36920969340018,-20.5535971721246,0.));
#9970=CARTESIAN_POINT('Ctrl Pts',(1.35165153211252,-20.6005007190809,0.));
#9971=CARTESIAN_POINT('Ctrl Pts',(1.3337902972259,-20.6473721041685,0.));
#9972=CARTESIAN_POINT('Ctrl Pts',(1.31562879653596,-20.694210454218,0.));
#9973=CARTESIAN_POINT('Ctrl Pts',(1.29717006491149,-20.7410149035348,0.));
#9974=CARTESIAN_POINT('Ctrl Pts',(1.27841722479261,-20.7877845975367,0.));
#9975=CARTESIAN_POINT('Ctrl Pts',(1.25937332001004,-20.83451869657,0.));
#9976=CARTESIAN_POINT('Ctrl Pts',(1.24004113517905,-20.881216381382,0.));
#9977=CARTESIAN_POINT('Ctrl Pts',(1.22042312071096,-20.9278768531175,0.));
#9978=CARTESIAN_POINT('Ctrl Pts',(1.20052150219502,-20.9744993243732,0.));
#9979=CARTESIAN_POINT('Ctrl Pts',(1.18033835060894,-21.0210830121673,0.));
#9980=CARTESIAN_POINT('Ctrl Pts',(1.15987566445807,-21.0676271313238,0.));
#9981=CARTESIAN_POINT('Ctrl Pts',(1.13913546246554,-21.1141308858087,0.));
#9982=CARTESIAN_POINT('Ctrl Pts',(1.11811982787746,-21.1605934684164,0.));
#9983=CARTESIAN_POINT('Ctrl Pts',(1.09683084929265,-21.2070140764156,0.));
#9984=CARTESIAN_POINT('Ctrl Pts',(1.07527058431887,-21.2533919248553,0.));
#9985=CARTESIAN_POINT('Ctrl Pts',(1.05344101900192,-21.2997262593683,0.));
#9986=CARTESIAN_POINT('Ctrl Pts',(1.03134402396952,-21.3460163737343,0.));
#9987=CARTESIAN_POINT('Ctrl Pts',(1.00898133629987,-21.3922616124166,0.));
#9988=CARTESIAN_POINT('Ctrl Pts',(0.986354611081129,-21.4384613333266,0.));
#9989=CARTESIAN_POINT('Ctrl Pts',(0.963465462815768,-21.4846148770804,0.));
#9990=CARTESIAN_POINT('Ctrl Pts',(0.940315509525146,-21.5307215366685,0.));
#9991=CARTESIAN_POINT('Ctrl Pts',(0.916906425150851,-21.5767805209408,0.));
#9992=CARTESIAN_POINT('Ctrl Pts',(0.89323996751367,-21.6227909401433,0.));
#9993=CARTESIAN_POINT('Ctrl Pts',(0.869317897714094,-21.6687518829182,0.));
#9994=CARTESIAN_POINT('Ctrl Pts',(0.845141916726555,-21.7146624809285,0.));
#9995=CARTESIAN_POINT('Ctrl Pts',(0.820713597934075,-21.7605219769118,0.));
#9996=CARTESIAN_POINT('Ctrl Pts',(0.796034321106407,-21.8063297959755,0.));
#9997=CARTESIAN_POINT('Ctrl Pts',(0.76611939168871,-21.8612367655148,0.));
#9998=CARTESIAN_POINT('Ctrl Pts',(0.740879090965094,-21.9069273598709,0.));
#9999=CARTESIAN_POINT('Ctrl Pts',(0.720488353007144,-21.9434380560096,0.));
#10000=CARTESIAN_POINT('Ctrl Pts',(0.705083756261754,-21.970797600548,0.));
#10001=CARTESIAN_POINT('Ctrl Pts',(0.694764450219577,-21.9890268624765,
0.));
#10002=CARTESIAN_POINT('',(0.69476445021964,-21.9890268624765,13.));
#10003=CARTESIAN_POINT('Ctrl Pts',(0.694764450219577,-21.9890268624765,
13.));
#10004=CARTESIAN_POINT('Ctrl Pts',(0.745561803311463,-21.89929231523,13.));
#10005=CARTESIAN_POINT('Ctrl Pts',(0.794921865619054,-21.8092529629783,
13.));
#10006=CARTESIAN_POINT('Ctrl Pts',(0.842819260998952,-21.7189137535649,
13.));
#10007=CARTESIAN_POINT('Ctrl Pts',(0.922187324214976,-21.569217762233,13.));
#10008=CARTESIAN_POINT('Ctrl Pts',(0.997528955778406,-21.4187072720354,
13.));
#10009=CARTESIAN_POINT('Ctrl Pts',(1.06858105435695,-21.2675022574599,13.));
#10010=CARTESIAN_POINT('Ctrl Pts',(1.12319586370563,-21.1512772168374,13.));
#10011=CARTESIAN_POINT('Ctrl Pts',(1.17527598698666,-21.0346391550274,13.));
#10012=CARTESIAN_POINT('Ctrl Pts',(1.22467603889823,-20.9176442421133,13.));
#10013=CARTESIAN_POINT('Ctrl Pts',(1.27785400463397,-20.7917020370051,13.));
#10014=CARTESIAN_POINT('Ctrl Pts',(1.32793259719133,-20.6653453730115,13.));
#10015=CARTESIAN_POINT('Ctrl Pts',(1.37465955747084,-20.5386490816447,13.));
#10016=CARTESIAN_POINT('Ctrl Pts',(1.40052887204096,-20.468506572981,13.));
#10017=CARTESIAN_POINT('Ctrl Pts',(1.42537603793014,-20.3982600553259,13.));
#10018=CARTESIAN_POINT('Ctrl Pts',(1.44915458926219,-20.3279233153994,13.));
#10019=CARTESIAN_POINT('Ctrl Pts',(1.47206853368884,-20.2601440748846,13.));
#10020=CARTESIAN_POINT('Ctrl Pts',(1.49398338587319,-20.1922811201552,13.));
#10021=CARTESIAN_POINT('Ctrl Pts',(1.51482335690232,-20.1243481792969,13.));
#10022=CARTESIAN_POINT('Ctrl Pts',(1.53283548327962,-20.0656332840501,13.));
#10023=CARTESIAN_POINT('Ctrl Pts',(1.55004791413554,-20.0068660725075,13.));
#10024=CARTESIAN_POINT('Ctrl Pts',(1.56645839123305,-19.9480555843418,13.));
#10025=CARTESIAN_POINT('Ctrl Pts',(1.57823544812775,-19.9058499579596,13.));
#10026=CARTESIAN_POINT('Ctrl Pts',(1.58960230205608,-19.8636220212356,13.));
#10027=CARTESIAN_POINT('Ctrl Pts',(1.60051957198611,-19.8213758753108,13.));
#10028=CARTESIAN_POINT('Ctrl Pts',(1.61125906786244,-19.7798176549079,13.));
#10029=CARTESIAN_POINT('Ctrl Pts',(1.62155711722061,-19.7382418852391,13.));
#10030=CARTESIAN_POINT('Ctrl Pts',(1.63136143467465,-19.6966529622227,13.));
#10031=CARTESIAN_POINT('Ctrl Pts',(1.63986235386958,-19.6605929227937,13.));
#10032=CARTESIAN_POINT('Ctrl Pts',(1.64798961240502,-19.6245230266729,13.));
#10033=CARTESIAN_POINT('Ctrl Pts',(1.65575861443972,-19.5884457884257,13.));
#10034=CARTESIAN_POINT('Ctrl Pts',(1.66279554775982,-19.5557680881516,13.));
#10035=CARTESIAN_POINT('Ctrl Pts',(1.66954412476468,-19.5230842956051,13.));
#10036=CARTESIAN_POINT('Ctrl Pts',(1.67602787914578,-19.49039635302,13.));
#10037=CARTESIAN_POINT('Ctrl Pts',(1.68148945136204,-19.462861756776,13.));
#10038=CARTESIAN_POINT('Ctrl Pts',(1.68676485585863,-19.4353241970144,13.));
#10039=CARTESIAN_POINT('Ctrl Pts',(1.69183425656632,-19.4077853970595,13.));
#10040=CARTESIAN_POINT('Ctrl Pts',(1.69917023100168,-19.3679337569745,13.));
#10041=CARTESIAN_POINT('Ctrl Pts',(1.70607400306928,-19.3280794803457,13.));
#10042=CARTESIAN_POINT('Ctrl Pts',(1.71232694131222,-19.2882303922902,13.));
#10043=CARTESIAN_POINT('Ctrl Pts',(1.71610520915756,-19.2641520274933,13.));
#10044=CARTESIAN_POINT('Ctrl Pts',(1.71964237041073,-19.2400756155396,13.));
#10045=CARTESIAN_POINT('Ctrl Pts',(1.72291205972096,-19.2160028181149,13.));
#10046=CARTESIAN_POINT('Ctrl Pts',(1.72592763308942,-19.1938009267636,13.));
#10047=CARTESIAN_POINT('Ctrl Pts',(1.7287143697234,-19.1716021264808,13.));
#10048=CARTESIAN_POINT('Ctrl Pts',(1.73129733456843,-19.1494073125539,13.));
#10049=CARTESIAN_POINT('Ctrl Pts',(1.73485046445803,-19.1188760968816,13.));
#10050=CARTESIAN_POINT('Ctrl Pts',(1.7380253099616,-19.0883522198199,13.));
#10051=CARTESIAN_POINT('Ctrl Pts',(1.74097263876108,-19.0578380260755,13.));
#10052=CARTESIAN_POINT('Ctrl Pts',(1.74284247673618,-19.0384792771458,13.));
#10053=CARTESIAN_POINT('Ctrl Pts',(1.74462241723582,-19.0191244316077,13.));
#10054=CARTESIAN_POINT('Ctrl Pts',(1.74632097575636,-18.9997750007207,13.));
#10055=CARTESIAN_POINT('Ctrl Pts',(1.74784535296742,-18.9824097871383,13.));
#10056=CARTESIAN_POINT('Ctrl Pts',(1.74930491161338,-18.9650489252781,13.));
#10057=CARTESIAN_POINT('Ctrl Pts',(1.75066513119224,-18.9476944344223,13.));
#10058=CARTESIAN_POINT('Ctrl Pts',(1.75209499287337,-18.9294514081815,13.));
#10059=CARTESIAN_POINT('Ctrl Pts',(1.75341524153271,-18.9112154259254,13.));
#10060=CARTESIAN_POINT('Ctrl Pts',(1.75452347864582,-18.8929901415011,13.));
#10061=CARTESIAN_POINT('Ctrl Pts',(1.75636425803994,-18.8627179843758,13.));
#10062=CARTESIAN_POINT('Ctrl Pts',(1.75761169393786,-18.8324756678787,13.));
#10063=CARTESIAN_POINT('Ctrl Pts',(1.75764008468136,-18.8022820950489,13.));
#10064=CARTESIAN_POINT('Ctrl Pts',(1.75765574034772,-18.785632284429,13.));
#10065=CARTESIAN_POINT('Ctrl Pts',(1.75729933637223,-18.7689972917426,13.));
#10066=CARTESIAN_POINT('Ctrl Pts',(1.75649392368161,-18.7523793044392,13.));
#10067=CARTESIAN_POINT('Ctrl Pts',(1.7558387619977,-18.7388614288561,13.));
#10068=CARTESIAN_POINT('Ctrl Pts',(1.75488656240343,-18.7253548001979,13.));
#10069=CARTESIAN_POINT('Ctrl Pts',(1.75362185428836,-18.7118598491961,13.));
#10070=CARTESIAN_POINT('',(0.69476445021964,-21.9890268624765,0.));
#10071=CARTESIAN_POINT('Origin',(-1.0097419586829E-27,-5.6665783176868E-12,
0.));
#10072=CARTESIAN_POINT('',(-0.694764450219586,-21.9890268624765,0.));
#10073=CARTESIAN_POINT('Origin',(-1.0097419586829E-27,-5.6665783176868E-12,
0.));
#10074=CARTESIAN_POINT('',(-0.694764450219586,-21.9890268624765,13.));
#10075=CARTESIAN_POINT('Origin',(-1.0097419586829E-27,-5.6665783176868E-12,
13.));
#10076=CARTESIAN_POINT('',(-0.694764450219586,-21.9890268624765,0.));
#10077=CARTESIAN_POINT('Ctrl Pts',(-1.75362185428837,-18.7118598491961,
0.));
#10078=CARTESIAN_POINT('Ctrl Pts',(-1.75362185428837,-18.7118598491961,
21.));
#10079=CARTESIAN_POINT('Ctrl Pts',(-1.75450132833464,-18.7212441956871,
0.));
#10080=CARTESIAN_POINT('Ctrl Pts',(-1.75450132833464,-18.7212441956871,
21.));
#10081=CARTESIAN_POINT('Ctrl Pts',(-1.75601041697575,-18.7400222442427,
0.));
#10082=CARTESIAN_POINT('Ctrl Pts',(-1.75601041697575,-18.7400222442427,
21.));
#10083=CARTESIAN_POINT('Ctrl Pts',(-1.75752447968136,-18.7682173836138,
0.));
#10084=CARTESIAN_POINT('Ctrl Pts',(-1.75752447968136,-18.7682173836138,
21.));
#10085=CARTESIAN_POINT('Ctrl Pts',(-1.7581175236483,-18.8058650094753,0.));
#10086=CARTESIAN_POINT('Ctrl Pts',(-1.7581175236483,-18.8058650094753,21.));
#10087=CARTESIAN_POINT('Ctrl Pts',(-1.75690876962598,-18.8530026395886,
0.));
#10088=CARTESIAN_POINT('Ctrl Pts',(-1.75690876962598,-18.8530026395886,
21.));
#10089=CARTESIAN_POINT('Ctrl Pts',(-1.75429229572776,-18.9002024267872,
0.));
#10090=CARTESIAN_POINT('Ctrl Pts',(-1.75429229572776,-18.9002024267872,
21.));
#10091=CARTESIAN_POINT('Ctrl Pts',(-1.75080409924534,-18.947447637865,0.));
#10092=CARTESIAN_POINT('Ctrl Pts',(-1.75080409924534,-18.947447637865,21.));
#10093=CARTESIAN_POINT('Ctrl Pts',(-1.74684309825013,-18.9947239970259,
0.));
#10094=CARTESIAN_POINT('Ctrl Pts',(-1.74684309825013,-18.9947239970259,
21.));
#10095=CARTESIAN_POINT('Ctrl Pts',(-1.74256297552949,-19.0420224296189,
0.));
#10096=CARTESIAN_POINT('Ctrl Pts',(-1.74256297552949,-19.0420224296189,
21.));
#10097=CARTESIAN_POINT('Ctrl Pts',(-1.73795301169841,-19.0893375576541,
0.));
#10098=CARTESIAN_POINT('Ctrl Pts',(-1.73795301169841,-19.0893375576541,
21.));
#10099=CARTESIAN_POINT('Ctrl Pts',(-1.73290313712354,-19.1366665585833,
0.));
#10100=CARTESIAN_POINT('Ctrl Pts',(-1.73290313712354,-19.1366665585833,
21.));
#10101=CARTESIAN_POINT('Ctrl Pts',(-1.72727220327098,-19.1840079312107,
0.));
#10102=CARTESIAN_POINT('Ctrl Pts',(-1.72727220327098,-19.1840079312107,
21.));
#10103=CARTESIAN_POINT('Ctrl Pts',(-1.72096104670234,-19.2313602042899,
0.));
#10104=CARTESIAN_POINT('Ctrl Pts',(-1.72096104670234,-19.2313602042899,
21.));
#10105=CARTESIAN_POINT('Ctrl Pts',(-1.71396454346262,-19.2787209722437,
0.));
#10106=CARTESIAN_POINT('Ctrl Pts',(-1.71396454346262,-19.2787209722437,
21.));
#10107=CARTESIAN_POINT('Ctrl Pts',(-1.70633457265124,-19.3260873558094,
0.));
#10108=CARTESIAN_POINT('Ctrl Pts',(-1.70633457265124,-19.3260873558094,
21.));
#10109=CARTESIAN_POINT('Ctrl Pts',(-1.69815571801252,-19.3734562555057,
0.));
#10110=CARTESIAN_POINT('Ctrl Pts',(-1.69815571801252,-19.3734562555057,
21.));
#10111=CARTESIAN_POINT('Ctrl Pts',(-1.68951753233571,-19.4208246682917,
0.));
#10112=CARTESIAN_POINT('Ctrl Pts',(-1.68951753233571,-19.4208246682917,
21.));
#10113=CARTESIAN_POINT('Ctrl Pts',(-1.68048476382294,-19.4681900187091,
0.));
#10114=CARTESIAN_POINT('Ctrl Pts',(-1.68048476382294,-19.4681900187091,
21.));
#10115=CARTESIAN_POINT('Ctrl Pts',(-1.67107974760949,-19.5155503513712,
0.));
#10116=CARTESIAN_POINT('Ctrl Pts',(-1.67107974760949,-19.5155503513712,
21.));
#10117=CARTESIAN_POINT('Ctrl Pts',(-1.66129908621006,-19.5629041190868,
0.));
#10118=CARTESIAN_POINT('Ctrl Pts',(-1.66129908621006,-19.5629041190868,
21.));
#10119=CARTESIAN_POINT('Ctrl Pts',(-1.65112409599283,-19.6102500448855,
0.));
#10120=CARTESIAN_POINT('Ctrl Pts',(-1.65112409599283,-19.6102500448855,
21.));
#10121=CARTESIAN_POINT('Ctrl Pts',(-1.64053294677822,-19.6575869645839,
0.));
#10122=CARTESIAN_POINT('Ctrl Pts',(-1.64053294677822,-19.6575869645839,
21.));
#10123=CARTESIAN_POINT('Ctrl Pts',(-1.62951389038422,-19.7049136553525,
0.));
#10124=CARTESIAN_POINT('Ctrl Pts',(-1.62951389038422,-19.7049136553525,
21.));
#10125=CARTESIAN_POINT('Ctrl Pts',(-1.61807191996834,-19.7522287462982,
0.));
#10126=CARTESIAN_POINT('Ctrl Pts',(-1.61807191996834,-19.7522287462982,
21.));
#10127=CARTESIAN_POINT('Ctrl Pts',(-1.60622162219699,-19.7995308006834,
0.));
#10128=CARTESIAN_POINT('Ctrl Pts',(-1.60622162219699,-19.7995308006834,
21.));
#10129=CARTESIAN_POINT('Ctrl Pts',(-1.59398289700559,-19.8468183626037,
0.));
#10130=CARTESIAN_POINT('Ctrl Pts',(-1.59398289700559,-19.8468183626037,
21.));
#10131=CARTESIAN_POINT('Ctrl Pts',(-1.58137589158952,-19.8940900137801,
0.));
#10132=CARTESIAN_POINT('Ctrl Pts',(-1.58137589158952,-19.8940900137801,
21.));
#10133=CARTESIAN_POINT('Ctrl Pts',(-1.56841542790453,-19.9413444362352,
0.));
#10134=CARTESIAN_POINT('Ctrl Pts',(-1.56841542790453,-19.9413444362352,
21.));
#10135=CARTESIAN_POINT('Ctrl Pts',(-1.55510860515914,-19.9885804375096,
0.));
#10136=CARTESIAN_POINT('Ctrl Pts',(-1.55510860515914,-19.9885804375096,
21.));
#10137=CARTESIAN_POINT('Ctrl Pts',(-1.54145790302918,-20.0357969106526,
0.));
#10138=CARTESIAN_POINT('Ctrl Pts',(-1.54145790302918,-20.0357969106526,
21.));
#10139=CARTESIAN_POINT('Ctrl Pts',(-1.52746305716965,-20.0829928089241,
0.));
#10140=CARTESIAN_POINT('Ctrl Pts',(-1.52746305716965,-20.0829928089241,
21.));
#10141=CARTESIAN_POINT('Ctrl Pts',(-1.51312326913583,-20.1301671167606,
0.));
#10142=CARTESIAN_POINT('Ctrl Pts',(-1.51312326913583,-20.1301671167606,
21.));
#10143=CARTESIAN_POINT('Ctrl Pts',(-1.49843965844502,-20.1773188177942,
0.));
#10144=CARTESIAN_POINT('Ctrl Pts',(-1.49843965844502,-20.1773188177942,
21.));
#10145=CARTESIAN_POINT('Ctrl Pts',(-1.48341623961914,-20.224446881308,0.));
#10146=CARTESIAN_POINT('Ctrl Pts',(-1.48341623961914,-20.224446881308,21.));
#10147=CARTESIAN_POINT('Ctrl Pts',(-1.46805861808021,-20.2715502770004,
0.));
#10148=CARTESIAN_POINT('Ctrl Pts',(-1.46805861808021,-20.2715502770004,
21.));
#10149=CARTESIAN_POINT('Ctrl Pts',(-1.45237321894404,-20.3186279833818,
0.));
#10150=CARTESIAN_POINT('Ctrl Pts',(-1.45237321894404,-20.3186279833818,
21.));
#10151=CARTESIAN_POINT('Ctrl Pts',(-1.43636637152782,-20.3656789980171,
0.));
#10152=CARTESIAN_POINT('Ctrl Pts',(-1.43636637152782,-20.3656789980171,
21.));
#10153=CARTESIAN_POINT('Ctrl Pts',(-1.4200432946371,-20.4127023494155,0.));
#10154=CARTESIAN_POINT('Ctrl Pts',(-1.4200432946371,-20.4127023494155,21.));
#10155=CARTESIAN_POINT('Ctrl Pts',(-1.40340771617025,-20.4596971004275,
0.));
#10156=CARTESIAN_POINT('Ctrl Pts',(-1.40340771617025,-20.4596971004275,
21.));
#10157=CARTESIAN_POINT('Ctrl Pts',(-1.38646244026049,-20.5066623390132,
0.));
#10158=CARTESIAN_POINT('Ctrl Pts',(-1.38646244026049,-20.5066623390132,
21.));
#10159=CARTESIAN_POINT('Ctrl Pts',(-1.36920969340018,-20.5535971721246,
0.));
#10160=CARTESIAN_POINT('Ctrl Pts',(-1.36920969340018,-20.5535971721246,
21.));
#10161=CARTESIAN_POINT('Ctrl Pts',(-1.35165153211253,-20.6005007190809,
0.));
#10162=CARTESIAN_POINT('Ctrl Pts',(-1.35165153211253,-20.6005007190809,
21.));
#10163=CARTESIAN_POINT('Ctrl Pts',(-1.33379029722591,-20.6473721041685,
0.));
#10164=CARTESIAN_POINT('Ctrl Pts',(-1.33379029722591,-20.6473721041685,
21.));
#10165=CARTESIAN_POINT('Ctrl Pts',(-1.31562879653597,-20.694210454218,0.));
#10166=CARTESIAN_POINT('Ctrl Pts',(-1.31562879653597,-20.694210454218,21.));
#10167=CARTESIAN_POINT('Ctrl Pts',(-1.2971700649115,-20.7410149035348,0.));
#10168=CARTESIAN_POINT('Ctrl Pts',(-1.2971700649115,-20.7410149035348,21.));
#10169=CARTESIAN_POINT('Ctrl Pts',(-1.27841722479262,-20.7877845975367,
0.));
#10170=CARTESIAN_POINT('Ctrl Pts',(-1.27841722479262,-20.7877845975367,
21.));
#10171=CARTESIAN_POINT('Ctrl Pts',(-1.25937332001005,-20.83451869657,0.));
#10172=CARTESIAN_POINT('Ctrl Pts',(-1.25937332001005,-20.83451869657,21.));
#10173=CARTESIAN_POINT('Ctrl Pts',(-1.24004113517906,-20.881216381382,0.));
#10174=CARTESIAN_POINT('Ctrl Pts',(-1.24004113517906,-20.881216381382,21.));
#10175=CARTESIAN_POINT('Ctrl Pts',(-1.22042312071097,-20.9278768531175,
0.));
#10176=CARTESIAN_POINT('Ctrl Pts',(-1.22042312071097,-20.9278768531175,
21.));
#10177=CARTESIAN_POINT('Ctrl Pts',(-1.20052150219503,-20.9744993243732,
0.));
#10178=CARTESIAN_POINT('Ctrl Pts',(-1.20052150219503,-20.9744993243732,
21.));
#10179=CARTESIAN_POINT('Ctrl Pts',(-1.18033835060895,-21.0210830121673,
0.));
#10180=CARTESIAN_POINT('Ctrl Pts',(-1.18033835060895,-21.0210830121673,
21.));
#10181=CARTESIAN_POINT('Ctrl Pts',(-1.15987566445808,-21.0676271313238,
0.));
#10182=CARTESIAN_POINT('Ctrl Pts',(-1.15987566445808,-21.0676271313238,
21.));
#10183=CARTESIAN_POINT('Ctrl Pts',(-1.13913546246555,-21.1141308858087,
0.));
#10184=CARTESIAN_POINT('Ctrl Pts',(-1.13913546246555,-21.1141308858087,
21.));
#10185=CARTESIAN_POINT('Ctrl Pts',(-1.11811982787747,-21.1605934684164,
0.));
#10186=CARTESIAN_POINT('Ctrl Pts',(-1.11811982787747,-21.1605934684164,
21.));
#10187=CARTESIAN_POINT('Ctrl Pts',(-1.09683084929266,-21.2070140764156,
0.));
#10188=CARTESIAN_POINT('Ctrl Pts',(-1.09683084929266,-21.2070140764156,
21.));
#10189=CARTESIAN_POINT('Ctrl Pts',(-1.07527058431887,-21.2533919248553,
0.));
#10190=CARTESIAN_POINT('Ctrl Pts',(-1.07527058431887,-21.2533919248553,
21.));
#10191=CARTESIAN_POINT('Ctrl Pts',(-1.05344101900192,-21.2997262593683,
0.));
#10192=CARTESIAN_POINT('Ctrl Pts',(-1.05344101900192,-21.2997262593683,
21.));
#10193=CARTESIAN_POINT('Ctrl Pts',(-1.03134402396953,-21.3460163737343,
0.));
#10194=CARTESIAN_POINT('Ctrl Pts',(-1.03134402396953,-21.3460163737343,
21.));
#10195=CARTESIAN_POINT('Ctrl Pts',(-1.00898133629988,-21.3922616124166,
0.));
#10196=CARTESIAN_POINT('Ctrl Pts',(-1.00898133629988,-21.3922616124166,
21.));
#10197=CARTESIAN_POINT('Ctrl Pts',(-0.986354611081139,-21.4384613333266,
0.));
#10198=CARTESIAN_POINT('Ctrl Pts',(-0.986354611081139,-21.4384613333266,
21.));
#10199=CARTESIAN_POINT('Ctrl Pts',(-0.963465462815776,-21.4846148770804,
0.));
#10200=CARTESIAN_POINT('Ctrl Pts',(-0.963465462815776,-21.4846148770804,
21.));
#10201=CARTESIAN_POINT('Ctrl Pts',(-0.940315509525156,-21.5307215366685,
0.));
#10202=CARTESIAN_POINT('Ctrl Pts',(-0.940315509525156,-21.5307215366685,
21.));
#10203=CARTESIAN_POINT('Ctrl Pts',(-0.916906425150857,-21.5767805209408,
0.));
#10204=CARTESIAN_POINT('Ctrl Pts',(-0.916906425150857,-21.5767805209408,
21.));
#10205=CARTESIAN_POINT('Ctrl Pts',(-0.893239967513677,-21.6227909401433,
0.));
#10206=CARTESIAN_POINT('Ctrl Pts',(-0.893239967513677,-21.6227909401433,
21.));
#10207=CARTESIAN_POINT('Ctrl Pts',(-0.869317897714105,-21.6687518829182,
0.));
#10208=CARTESIAN_POINT('Ctrl Pts',(-0.869317897714105,-21.6687518829182,
21.));
#10209=CARTESIAN_POINT('Ctrl Pts',(-0.845141916726563,-21.7146624809285,
0.));
#10210=CARTESIAN_POINT('Ctrl Pts',(-0.845141916726563,-21.7146624809285,
21.));
#10211=CARTESIAN_POINT('Ctrl Pts',(-0.820713597934081,-21.7605219769118,
0.));
#10212=CARTESIAN_POINT('Ctrl Pts',(-0.820713597934081,-21.7605219769118,
21.));
#10213=CARTESIAN_POINT('Ctrl Pts',(-0.796034321106418,-21.8063297959755,
0.));
#10214=CARTESIAN_POINT('Ctrl Pts',(-0.796034321106418,-21.8063297959755,
21.));
#10215=CARTESIAN_POINT('Ctrl Pts',(-0.771105213258335,-21.8520856039249,
0.));
#10216=CARTESIAN_POINT('Ctrl Pts',(-0.771105213258335,-21.8520856039249,
21.));
#10217=CARTESIAN_POINT('Ctrl Pts',(-0.745927151109825,-21.8977892409997,
0.));
#10218=CARTESIAN_POINT('Ctrl Pts',(-0.745927151109825,-21.8977892409997,
21.));
#10219=CARTESIAN_POINT('Ctrl Pts',(-0.725586037496641,-21.9343103819749,
0.));
#10220=CARTESIAN_POINT('Ctrl Pts',(-0.725586037496641,-21.9343103819749,
21.));
#10221=CARTESIAN_POINT('Ctrl Pts',(-0.71021862184356,-21.9616777523685,
0.));
#10222=CARTESIAN_POINT('Ctrl Pts',(-0.71021862184356,-21.9616777523685,
21.));
#10223=CARTESIAN_POINT('Ctrl Pts',(-0.699924103234227,-21.9799122315157,
0.));
#10224=CARTESIAN_POINT('Ctrl Pts',(-0.699924103234227,-21.9799122315157,
21.));
#10225=CARTESIAN_POINT('Ctrl Pts',(-0.694764450219586,-21.9890268624765,
0.));
#10226=CARTESIAN_POINT('Ctrl Pts',(-0.694764450219586,-21.9890268624765,
21.));
#10227=CARTESIAN_POINT('Ctrl Pts',(-1.75362185428837,-18.7118598491961,
0.));
#10228=CARTESIAN_POINT('Ctrl Pts',(-1.75450132833464,-18.7212441956871,
0.));
#10229=CARTESIAN_POINT('Ctrl Pts',(-1.75601041697575,-18.7400222442427,
0.));
#10230=CARTESIAN_POINT('Ctrl Pts',(-1.75752447968136,-18.7682173836138,
0.));
#10231=CARTESIAN_POINT('Ctrl Pts',(-1.7581175236483,-18.8058650094753,0.));
#10232=CARTESIAN_POINT('Ctrl Pts',(-1.75690876962598,-18.8530026395886,
0.));
#10233=CARTESIAN_POINT('Ctrl Pts',(-1.75429229572776,-18.9002024267872,
0.));
#10234=CARTESIAN_POINT('Ctrl Pts',(-1.75080409924534,-18.947447637865,0.));
#10235=CARTESIAN_POINT('Ctrl Pts',(-1.74684309825013,-18.9947239970259,
0.));
#10236=CARTESIAN_POINT('Ctrl Pts',(-1.74256297552949,-19.0420224296189,
0.));
#10237=CARTESIAN_POINT('Ctrl Pts',(-1.73795301169841,-19.0893375576541,
0.));
#10238=CARTESIAN_POINT('Ctrl Pts',(-1.73290313712354,-19.1366665585833,
0.));
#10239=CARTESIAN_POINT('Ctrl Pts',(-1.72727220327098,-19.1840079312107,
0.));
#10240=CARTESIAN_POINT('Ctrl Pts',(-1.72096104670234,-19.2313602042899,
0.));
#10241=CARTESIAN_POINT('Ctrl Pts',(-1.71396454346262,-19.2787209722437,
0.));
#10242=CARTESIAN_POINT('Ctrl Pts',(-1.70633457265124,-19.3260873558094,
0.));
#10243=CARTESIAN_POINT('Ctrl Pts',(-1.69815571801252,-19.3734562555057,
0.));
#10244=CARTESIAN_POINT('Ctrl Pts',(-1.68951753233571,-19.4208246682917,
0.));
#10245=CARTESIAN_POINT('Ctrl Pts',(-1.68048476382294,-19.4681900187091,
0.));
#10246=CARTESIAN_POINT('Ctrl Pts',(-1.67107974760949,-19.5155503513712,
0.));
#10247=CARTESIAN_POINT('Ctrl Pts',(-1.66129908621006,-19.5629041190868,
0.));
#10248=CARTESIAN_POINT('Ctrl Pts',(-1.65112409599283,-19.6102500448855,
0.));
#10249=CARTESIAN_POINT('Ctrl Pts',(-1.64053294677822,-19.6575869645839,
0.));
#10250=CARTESIAN_POINT('Ctrl Pts',(-1.62951389038422,-19.7049136553525,
0.));
#10251=CARTESIAN_POINT('Ctrl Pts',(-1.61807191996834,-19.7522287462982,
0.));
#10252=CARTESIAN_POINT('Ctrl Pts',(-1.60622162219699,-19.7995308006834,
0.));
#10253=CARTESIAN_POINT('Ctrl Pts',(-1.59398289700559,-19.8468183626037,
0.));
#10254=CARTESIAN_POINT('Ctrl Pts',(-1.58137589158952,-19.8940900137801,
0.));
#10255=CARTESIAN_POINT('Ctrl Pts',(-1.56841542790453,-19.9413444362352,
0.));
#10256=CARTESIAN_POINT('Ctrl Pts',(-1.55510860515914,-19.9885804375096,
0.));
#10257=CARTESIAN_POINT('Ctrl Pts',(-1.54145790302918,-20.0357969106526,
0.));
#10258=CARTESIAN_POINT('Ctrl Pts',(-1.52746305716965,-20.0829928089241,
0.));
#10259=CARTESIAN_POINT('Ctrl Pts',(-1.51312326913583,-20.1301671167606,
0.));
#10260=CARTESIAN_POINT('Ctrl Pts',(-1.49843965844502,-20.1773188177942,
0.));
#10261=CARTESIAN_POINT('Ctrl Pts',(-1.48341623961914,-20.224446881308,0.));
#10262=CARTESIAN_POINT('Ctrl Pts',(-1.46805861808021,-20.2715502770004,
0.));
#10263=CARTESIAN_POINT('Ctrl Pts',(-1.45237321894404,-20.3186279833818,
0.));
#10264=CARTESIAN_POINT('Ctrl Pts',(-1.43636637152782,-20.3656789980171,
0.));
#10265=CARTESIAN_POINT('Ctrl Pts',(-1.4200432946371,-20.4127023494155,0.));
#10266=CARTESIAN_POINT('Ctrl Pts',(-1.40340771617025,-20.4596971004275,
0.));
#10267=CARTESIAN_POINT('Ctrl Pts',(-1.38646244026049,-20.5066623390132,
0.));
#10268=CARTESIAN_POINT('Ctrl Pts',(-1.36920969340018,-20.5535971721246,
0.));
#10269=CARTESIAN_POINT('Ctrl Pts',(-1.35165153211253,-20.6005007190809,
0.));
#10270=CARTESIAN_POINT('Ctrl Pts',(-1.33379029722591,-20.6473721041685,
0.));
#10271=CARTESIAN_POINT('Ctrl Pts',(-1.31562879653597,-20.694210454218,0.));
#10272=CARTESIAN_POINT('Ctrl Pts',(-1.2971700649115,-20.7410149035348,0.));
#10273=CARTESIAN_POINT('Ctrl Pts',(-1.27841722479262,-20.7877845975367,
0.));
#10274=CARTESIAN_POINT('Ctrl Pts',(-1.25937332001005,-20.83451869657,0.));
#10275=CARTESIAN_POINT('Ctrl Pts',(-1.24004113517906,-20.881216381382,0.));
#10276=CARTESIAN_POINT('Ctrl Pts',(-1.22042312071097,-20.9278768531175,
0.));
#10277=CARTESIAN_POINT('Ctrl Pts',(-1.20052150219503,-20.9744993243732,
0.));
#10278=CARTESIAN_POINT('Ctrl Pts',(-1.18033835060895,-21.0210830121673,
0.));
#10279=CARTESIAN_POINT('Ctrl Pts',(-1.15987566445808,-21.0676271313238,
0.));
#10280=CARTESIAN_POINT('Ctrl Pts',(-1.13913546246555,-21.1141308858087,
0.));
#10281=CARTESIAN_POINT('Ctrl Pts',(-1.11811982787747,-21.1605934684164,
0.));
#10282=CARTESIAN_POINT('Ctrl Pts',(-1.09683084929266,-21.2070140764156,
0.));
#10283=CARTESIAN_POINT('Ctrl Pts',(-1.07527058431887,-21.2533919248553,
0.));
#10284=CARTESIAN_POINT('Ctrl Pts',(-1.05344101900192,-21.2997262593683,
0.));
#10285=CARTESIAN_POINT('Ctrl Pts',(-1.03134402396953,-21.3460163737343,
0.));
#10286=CARTESIAN_POINT('Ctrl Pts',(-1.00898133629988,-21.3922616124166,
0.));
#10287=CARTESIAN_POINT('Ctrl Pts',(-0.986354611081139,-21.4384613333266,
0.));
#10288=CARTESIAN_POINT('Ctrl Pts',(-0.963465462815776,-21.4846148770804,
0.));
#10289=CARTESIAN_POINT('Ctrl Pts',(-0.940315509525156,-21.5307215366685,
0.));
#10290=CARTESIAN_POINT('Ctrl Pts',(-0.916906425150857,-21.5767805209408,
0.));
#10291=CARTESIAN_POINT('Ctrl Pts',(-0.893239967513677,-21.6227909401433,
0.));
#10292=CARTESIAN_POINT('Ctrl Pts',(-0.869317897714105,-21.6687518829182,
0.));
#10293=CARTESIAN_POINT('Ctrl Pts',(-0.845141916726563,-21.7146624809285,
0.));
#10294=CARTESIAN_POINT('Ctrl Pts',(-0.820713597934081,-21.7605219769118,
0.));
#10295=CARTESIAN_POINT('Ctrl Pts',(-0.796034321106418,-21.8063297959755,
0.));
#10296=CARTESIAN_POINT('Ctrl Pts',(-0.766119391688718,-21.8612367655148,
0.));
#10297=CARTESIAN_POINT('Ctrl Pts',(-0.740879090965101,-21.9069273598709,
0.));
#10298=CARTESIAN_POINT('Ctrl Pts',(-0.720488353007154,-21.9434380560096,
0.));
#10299=CARTESIAN_POINT('Ctrl Pts',(-0.705083756261763,-21.970797600548,
0.));
#10300=CARTESIAN_POINT('Ctrl Pts',(-0.694764450219586,-21.9890268624765,
0.));
#10301=CARTESIAN_POINT('Ctrl Pts',(-1.75362185428837,-18.7118598491961,
13.));
#10302=CARTESIAN_POINT('Ctrl Pts',(-1.75510417082366,-18.7276767707249,
13.));
#10303=CARTESIAN_POINT('Ctrl Pts',(-1.75615601189424,-18.743509767289,13.));
#10304=CARTESIAN_POINT('Ctrl Pts',(-1.75680608702495,-18.7593580381833,
13.));
#10305=CARTESIAN_POINT('Ctrl Pts',(-1.75756802370039,-18.7779333970397,
13.));
#10306=CARTESIAN_POINT('Ctrl Pts',(-1.75777887919059,-18.7965297250683,
13.));
#10307=CARTESIAN_POINT('Ctrl Pts',(-1.75755628860694,-18.8151436576357,
13.));
#10308=CARTESIAN_POINT('Ctrl Pts',(-1.75724309300303,-18.841334351581,13.));
#10309=CARTESIAN_POINT('Ctrl Pts',(-1.75607893899588,-18.8675597701101,
13.));
#10310=CARTESIAN_POINT('Ctrl Pts',(-1.75447363677663,-18.8938074357167,
13.));
#10311=CARTESIAN_POINT('Ctrl Pts',(-1.75340585762642,-18.9112662729005,
13.));
#10312=CARTESIAN_POINT('Ctrl Pts',(-1.75214492935969,-18.9287348768864,
13.));
#10313=CARTESIAN_POINT('Ctrl Pts',(-1.75078122387605,-18.9462100283318,
13.));
#10314=CARTESIAN_POINT('Ctrl Pts',(-1.74934570031115,-18.9646054898159,
13.));
#10315=CARTESIAN_POINT('Ctrl Pts',(-1.74779717198844,-18.9830081805071,
13.));
#10316=CARTESIAN_POINT('Ctrl Pts',(-1.74617674699282,-19.0014156957804,
13.));
#10317=CARTESIAN_POINT('Ctrl Pts',(-1.74437717633237,-19.0218582491274,
13.));
#10318=CARTESIAN_POINT('Ctrl Pts',(-1.74248762596055,-19.0423067706055,
13.));
#10319=CARTESIAN_POINT('Ctrl Pts',(-1.74049525500399,-19.0627595477289,
13.));
#10320=CARTESIAN_POINT('Ctrl Pts',(-1.73749165908531,-19.093593101938,13.));
#10321=CARTESIAN_POINT('Ctrl Pts',(-1.73424805120509,-19.1244363539499,
13.));
#10322=CARTESIAN_POINT('Ctrl Pts',(-1.73060838684927,-19.155287003772,13.));
#10323=CARTESIAN_POINT('Ctrl Pts',(-1.72796425026603,-19.177699326403,13.));
#10324=CARTESIAN_POINT('Ctrl Pts',(-1.72510779282446,-19.2001156538051,
13.));
#10325=CARTESIAN_POINT('Ctrl Pts',(-1.72201836571179,-19.2225350169884,
13.));
#10326=CARTESIAN_POINT('Ctrl Pts',(-1.71824180560906,-19.2499407687471,
13.));
#10327=CARTESIAN_POINT('Ctrl Pts',(-1.71411839343755,-19.2773510352525,
13.));
#10328=CARTESIAN_POINT('Ctrl Pts',(-1.70969587297323,-19.3047632983646,
13.));
#10329=CARTESIAN_POINT('Ctrl Pts',(-1.70491881688378,-19.3343730920291,
13.));
#10330=CARTESIAN_POINT('Ctrl Pts',(-1.69979875336634,-19.3639851445184,
13.));
#10331=CARTESIAN_POINT('Ctrl Pts',(-1.69442732753457,-19.3935962281315,
13.));
#10332=CARTESIAN_POINT('Ctrl Pts',(-1.68946845243803,-19.42093304143,13.));
#10333=CARTESIAN_POINT('Ctrl Pts',(-1.68429785630297,-19.4482690053405,
13.));
#10334=CARTESIAN_POINT('Ctrl Pts',(-1.67894398812104,-19.4756022976176,
13.));
#10335=CARTESIAN_POINT('Ctrl Pts',(-1.67167048330012,-19.512735978611,13.));
#10336=CARTESIAN_POINT('Ctrl Pts',(-1.66405675112383,-19.5498647402118,
13.));
#10337=CARTESIAN_POINT('Ctrl Pts',(-1.65607285223162,-19.5869856493823,
13.));
#10338=CARTESIAN_POINT('Ctrl Pts',(-1.64836856223834,-19.6228065249877,
13.));
#10339=CARTESIAN_POINT('Ctrl Pts',(-1.64031177032937,-19.6586201923391,
13.));
#10340=CARTESIAN_POINT('Ctrl Pts',(-1.63188637919459,-19.6944241981031,
13.));
#10341=CARTESIAN_POINT('Ctrl Pts',(-1.62044024925903,-19.7430649431597,
13.));
#10342=CARTESIAN_POINT('Ctrl Pts',(-1.60831707818776,-19.7916877990303,
13.));
#10343=CARTESIAN_POINT('Ctrl Pts',(-1.59560243914448,-19.8402857465804,
13.));
#10344=CARTESIAN_POINT('Ctrl Pts',(-1.58442654783662,-19.8830022859769,
13.));
#10345=CARTESIAN_POINT('Ctrl Pts',(-1.57280052806414,-19.9256995150004,
13.));
#10346=CARTESIAN_POINT('Ctrl Pts',(-1.56075644051379,-19.9683733417535,
13.));
#10347=CARTESIAN_POINT('Ctrl Pts',(-1.54300053140843,-20.0312849227129,
13.));
#10348=CARTESIAN_POINT('Ctrl Pts',(-1.52432694531153,-20.0941457150648,
13.));
#10349=CARTESIAN_POINT('Ctrl Pts',(-1.50474000380958,-20.1569447711145,
13.));
#10350=CARTESIAN_POINT('Ctrl Pts',(-1.48002109248255,-20.2361977927135,
13.));
#10351=CARTESIAN_POINT('Ctrl Pts',(-1.45385270859109,-20.3153523891039,
13.));
#10352=CARTESIAN_POINT('Ctrl Pts',(-1.42635858929742,-20.3943871109086,
13.));
#10353=CARTESIAN_POINT('Ctrl Pts',(-1.38911568501702,-20.5014457348841,
13.));
#10354=CARTESIAN_POINT('Ctrl Pts',(-1.34943433501594,-20.6082844520166,
13.));
#10355=CARTESIAN_POINT('Ctrl Pts',(-1.30744723531062,-20.7148563913857,
13.));
#10356=CARTESIAN_POINT('Ctrl Pts',(-1.27001463635412,-20.8098680662672,
13.));
#10357=CARTESIAN_POINT('Ctrl Pts',(-1.23075788105027,-20.9046675821832,
13.));
#10358=CARTESIAN_POINT('Ctrl Pts',(-1.18977154269178,-20.9992246142304,
13.));
#10359=CARTESIAN_POINT('Ctrl Pts',(-1.1316826302001,-21.1332379313512,13.));
#10360=CARTESIAN_POINT('Ctrl Pts',(-1.07011397706108,-21.2667633195663,
13.));
#10361=CARTESIAN_POINT('Ctrl Pts',(-1.00527632047501,-21.3997200780868,
13.));
#10362=CARTESIAN_POINT('Ctrl Pts',(-0.954911968701506,-21.5029977304476,
13.));
#10363=CARTESIAN_POINT('Ctrl Pts',(-0.902570955454164,-21.6059349895582,
13.));
#10364=CARTESIAN_POINT('Ctrl Pts',(-0.848338494601997,-21.7084903372331,
13.));
#10365=CARTESIAN_POINT('Ctrl Pts',(-0.801423317792771,-21.7972084627486,
13.));
#10366=CARTESIAN_POINT('Ctrl Pts',(-0.753096147909189,-21.8856382928766,
13.));
#10367=CARTESIAN_POINT('Ctrl Pts',(-0.703383282402061,-21.9737740855816,
13.));
#10368=CARTESIAN_POINT('Ctrl Pts',(-0.700514964339855,-21.9788593182183,
13.));
#10369=CARTESIAN_POINT('Ctrl Pts',(-0.697642020192887,-21.9839435771672,
13.));
#10370=CARTESIAN_POINT('Ctrl Pts',(-0.694764450219586,-21.9890268624765,
13.));
#10371=CARTESIAN_POINT('Ctrl Pts',(-6.13422273260091,-21.1275013067528,
0.));
#10372=CARTESIAN_POINT('Ctrl Pts',(-6.13422273260091,-21.1275013067528,
21.));
#10373=CARTESIAN_POINT('Ctrl Pts',(-6.12649903511518,-21.1204271980506,
0.));
#10374=CARTESIAN_POINT('Ctrl Pts',(-6.12649903511518,-21.1204271980506,
21.));
#10375=CARTESIAN_POINT('Ctrl Pts',(-6.11107360216958,-21.1062663590356,
0.));
#10376=CARTESIAN_POINT('Ctrl Pts',(-6.11107360216958,-21.1062663590356,
21.));
#10377=CARTESIAN_POINT('Ctrl Pts',(-6.08800133883115,-21.0849872356853,
0.));
#10378=CARTESIAN_POINT('Ctrl Pts',(-6.08800133883115,-21.0849872356853,
21.));
#10379=CARTESIAN_POINT('Ctrl Pts',(-6.05737013696533,-21.0565393163693,
0.));
#10380=CARTESIAN_POINT('Ctrl Pts',(-6.05737013696533,-21.0565393163693,
21.));
#10381=CARTESIAN_POINT('Ctrl Pts',(-6.01930117633045,-21.0208530236003,
0.));
#10382=CARTESIAN_POINT('Ctrl Pts',(-6.01930117633045,-21.0208530236003,
21.));
#10383=CARTESIAN_POINT('Ctrl Pts',(-5.98145286361837,-20.9850401822713,
0.));
#10384=CARTESIAN_POINT('Ctrl Pts',(-5.98145286361837,-20.9850401822713,
21.));
#10385=CARTESIAN_POINT('Ctrl Pts',(-5.94382608200804,-20.9491006734021,
0.));
#10386=CARTESIAN_POINT('Ctrl Pts',(-5.94382608200804,-20.9491006734021,
21.));
#10387=CARTESIAN_POINT('Ctrl Pts',(-5.906422006626,-20.9130344665641,0.));
#10388=CARTESIAN_POINT('Ctrl Pts',(-5.906422006626,-20.9130344665641,21.));
#10389=CARTESIAN_POINT('Ctrl Pts',(-5.86924212736288,-20.8768416821402,
0.));
#10390=CARTESIAN_POINT('Ctrl Pts',(-5.86924212736288,-20.8768416821402,
21.));
#10391=CARTESIAN_POINT('Ctrl Pts',(-5.83228817460178,-20.8405225541277,
0.));
#10392=CARTESIAN_POINT('Ctrl Pts',(-5.83228817460178,-20.8405225541277,
21.));
#10393=CARTESIAN_POINT('Ctrl Pts',(-5.79556203439644,-20.8040773827343,
0.));
#10394=CARTESIAN_POINT('Ctrl Pts',(-5.79556203439644,-20.8040773827343,
21.));
#10395=CARTESIAN_POINT('Ctrl Pts',(-5.75906566327796,-20.7675064905026,
0.));
#10396=CARTESIAN_POINT('Ctrl Pts',(-5.75906566327796,-20.7675064905026,
21.));
#10397=CARTESIAN_POINT('Ctrl Pts',(-5.72280100798241,-20.7308101804425,
0.));
#10398=CARTESIAN_POINT('Ctrl Pts',(-5.72280100798241,-20.7308101804425,
21.));
#10399=CARTESIAN_POINT('Ctrl Pts',(-5.68676990500164,-20.6939886877061,
0.));
#10400=CARTESIAN_POINT('Ctrl Pts',(-5.68676990500164,-20.6939886877061,
21.));
#10401=CARTESIAN_POINT('Ctrl Pts',(-5.65097411164335,-20.6570421847033,
0.));
#10402=CARTESIAN_POINT('Ctrl Pts',(-5.65097411164335,-20.6570421847033,
21.));
#10403=CARTESIAN_POINT('Ctrl Pts',(-5.6154153671515,-20.6199707996366,0.));
#10404=CARTESIAN_POINT('Ctrl Pts',(-5.6154153671515,-20.6199707996366,21.));
#10405=CARTESIAN_POINT('Ctrl Pts',(-5.58009544402475,-20.5827746317185,
0.));
#10406=CARTESIAN_POINT('Ctrl Pts',(-5.58009544402475,-20.5827746317185,
21.));
#10407=CARTESIAN_POINT('Ctrl Pts',(-5.5450161968946,-20.5454537676144,0.));
#10408=CARTESIAN_POINT('Ctrl Pts',(-5.5450161968946,-20.5454537676144,21.));
#10409=CARTESIAN_POINT('Ctrl Pts',(-5.51017962306782,-20.5080083009242,
0.));
#10410=CARTESIAN_POINT('Ctrl Pts',(-5.51017962306782,-20.5080083009242,
21.));
#10411=CARTESIAN_POINT('Ctrl Pts',(-5.47558784449851,-20.4704383353718,
0.));
#10412=CARTESIAN_POINT('Ctrl Pts',(-5.47558784449851,-20.4704383353718,
21.));
#10413=CARTESIAN_POINT('Ctrl Pts',(-5.44124306065111,-20.4327439816542,
0.));
#10414=CARTESIAN_POINT('Ctrl Pts',(-5.44124306065111,-20.4327439816542,
21.));
#10415=CARTESIAN_POINT('Ctrl Pts',(-5.40714750595875,-20.3949253578015,
0.));
#10416=CARTESIAN_POINT('Ctrl Pts',(-5.40714750595875,-20.3949253578015,
21.));
#10417=CARTESIAN_POINT('Ctrl Pts',(-5.37330341114649,-20.3569825877537,
0.));
#10418=CARTESIAN_POINT('Ctrl Pts',(-5.37330341114649,-20.3569825877537,
21.));
#10419=CARTESIAN_POINT('Ctrl Pts',(-5.33971294212214,-20.3189158047642,
0.));
#10420=CARTESIAN_POINT('Ctrl Pts',(-5.33971294212214,-20.3189158047642,
21.));
#10421=CARTESIAN_POINT('Ctrl Pts',(-5.30637824220998,-20.2807251380077,
0.));
#10422=CARTESIAN_POINT('Ctrl Pts',(-5.30637824220998,-20.2807251380077,
21.));
#10423=CARTESIAN_POINT('Ctrl Pts',(-5.27330152298151,-20.2424106921768,
0.));
#10424=CARTESIAN_POINT('Ctrl Pts',(-5.27330152298151,-20.2424106921768,
21.));
#10425=CARTESIAN_POINT('Ctrl Pts',(-5.24048514441891,-20.2039725283917,
0.));
#10426=CARTESIAN_POINT('Ctrl Pts',(-5.24048514441891,-20.2039725283917,
21.));
#10427=CARTESIAN_POINT('Ctrl Pts',(-5.20793168386164,-20.1654106491899,
0.));
#10428=CARTESIAN_POINT('Ctrl Pts',(-5.20793168386164,-20.1654106491899,
21.));
#10429=CARTESIAN_POINT('Ctrl Pts',(-5.17564404279922,-20.1267249732337,
0.));
#10430=CARTESIAN_POINT('Ctrl Pts',(-5.17564404279922,-20.1267249732337,
21.));
#10431=CARTESIAN_POINT('Ctrl Pts',(-5.14362537555398,-20.087915358486,0.));
#10432=CARTESIAN_POINT('Ctrl Pts',(-5.14362537555398,-20.087915358486,21.));
#10433=CARTESIAN_POINT('Ctrl Pts',(-5.11187891582335,-20.0489816528155,
0.));
#10434=CARTESIAN_POINT('Ctrl Pts',(-5.11187891582335,-20.0489816528155,
21.));
#10435=CARTESIAN_POINT('Ctrl Pts',(-5.08040781745337,-20.0099237417205,
0.));
#10436=CARTESIAN_POINT('Ctrl Pts',(-5.08040781745337,-20.0099237417205,
21.));
#10437=CARTESIAN_POINT('Ctrl Pts',(-5.04921502064063,-19.9707415879783,
0.));
#10438=CARTESIAN_POINT('Ctrl Pts',(-5.04921502064063,-19.9707415879783,
21.));
#10439=CARTESIAN_POINT('Ctrl Pts',(-5.01830302225558,-19.931435301086,0.));
#10440=CARTESIAN_POINT('Ctrl Pts',(-5.01830302225558,-19.931435301086,21.));
#10441=CARTESIAN_POINT('Ctrl Pts',(-4.98767405031333,-19.8920050831202,
0.));
#10442=CARTESIAN_POINT('Ctrl Pts',(-4.98767405031333,-19.8920050831202,
21.));
#10443=CARTESIAN_POINT('Ctrl Pts',(-4.95733049830096,-19.8524510953961,
0.));
#10444=CARTESIAN_POINT('Ctrl Pts',(-4.95733049830096,-19.8524510953961,
21.));
#10445=CARTESIAN_POINT('Ctrl Pts',(-4.92727531494347,-19.8127733387903,
0.));
#10446=CARTESIAN_POINT('Ctrl Pts',(-4.92727531494347,-19.8127733387903,
21.));
#10447=CARTESIAN_POINT('Ctrl Pts',(-4.89751233527805,-19.772971552601,0.));
#10448=CARTESIAN_POINT('Ctrl Pts',(-4.89751233527805,-19.772971552601,21.));
#10449=CARTESIAN_POINT('Ctrl Pts',(-4.86804682289087,-19.7330450480715,
0.));
#10450=CARTESIAN_POINT('Ctrl Pts',(-4.86804682289087,-19.7330450480715,
21.));
#10451=CARTESIAN_POINT('Ctrl Pts',(-4.83888510708974,-19.6929928227072,
0.));
#10452=CARTESIAN_POINT('Ctrl Pts',(-4.83888510708974,-19.6929928227072,
21.));
#10453=CARTESIAN_POINT('Ctrl Pts',(-4.81003361418061,-19.6528138625329,
0.));
#10454=CARTESIAN_POINT('Ctrl Pts',(-4.81003361418061,-19.6528138625329,
21.));
#10455=CARTESIAN_POINT('Ctrl Pts',(-4.78149799361731,-19.6125074152527,
0.));
#10456=CARTESIAN_POINT('Ctrl Pts',(-4.78149799361731,-19.6125074152527,
21.));
#10457=CARTESIAN_POINT('Ctrl Pts',(-4.75328238194611,-19.5720732205813,
0.));
#10458=CARTESIAN_POINT('Ctrl Pts',(-4.75328238194611,-19.5720732205813,
21.));
#10459=CARTESIAN_POINT('Ctrl Pts',(-4.72538815796616,-19.531511899192,0.));
#10460=CARTESIAN_POINT('Ctrl Pts',(-4.72538815796616,-19.531511899192,21.));
#10461=CARTESIAN_POINT('Ctrl Pts',(-4.69781487613785,-19.4908246636763,
0.));
#10462=CARTESIAN_POINT('Ctrl Pts',(-4.69781487613785,-19.4908246636763,
21.));
#10463=CARTESIAN_POINT('Ctrl Pts',(-4.67056260851454,-19.4500125912299,
0.));
#10464=CARTESIAN_POINT('Ctrl Pts',(-4.67056260851454,-19.4500125912299,
21.));
#10465=CARTESIAN_POINT('Ctrl Pts',(-4.64363405547472,-19.4090759683639,
0.));
#10466=CARTESIAN_POINT('Ctrl Pts',(-4.64363405547472,-19.4090759683639,
21.));
#10467=CARTESIAN_POINT('Ctrl Pts',(-4.61703633725712,-19.3680137353983,
0.));
#10468=CARTESIAN_POINT('Ctrl Pts',(-4.61703633725712,-19.3680137353983,
21.));
#10469=CARTESIAN_POINT('Ctrl Pts',(-4.59078395765677,-19.3268225655679,
0.));
#10470=CARTESIAN_POINT('Ctrl Pts',(-4.59078395765677,-19.3268225655679,
21.));
#10471=CARTESIAN_POINT('Ctrl Pts',(-4.56489651606741,-19.2854975819105,
0.));
#10472=CARTESIAN_POINT('Ctrl Pts',(-4.56489651606741,-19.2854975819105,
21.));
#10473=CARTESIAN_POINT('Ctrl Pts',(-4.53939338835152,-19.2440340196551,
0.));
#10474=CARTESIAN_POINT('Ctrl Pts',(-4.53939338835152,-19.2440340196551,
21.));
#10475=CARTESIAN_POINT('Ctrl Pts',(-4.51428889122955,-19.2024287376926,
0.));
#10476=CARTESIAN_POINT('Ctrl Pts',(-4.51428889122955,-19.2024287376926,
21.));
#10477=CARTESIAN_POINT('Ctrl Pts',(-4.48958819710577,-19.1606814968494,
0.));
#10478=CARTESIAN_POINT('Ctrl Pts',(-4.48958819710577,-19.1606814968494,
21.));
#10479=CARTESIAN_POINT('Ctrl Pts',(-4.46528051067022,-19.1187970904932,
0.));
#10480=CARTESIAN_POINT('Ctrl Pts',(-4.46528051067022,-19.1187970904932,
21.));
#10481=CARTESIAN_POINT('Ctrl Pts',(-4.44134542994082,-19.0767833717249,
0.));
#10482=CARTESIAN_POINT('Ctrl Pts',(-4.44134542994082,-19.0767833717249,
21.));
#10483=CARTESIAN_POINT('Ctrl Pts',(-4.41776558033332,-19.034647328575,0.));
#10484=CARTESIAN_POINT('Ctrl Pts',(-4.41776558033332,-19.034647328575,21.));
#10485=CARTESIAN_POINT('Ctrl Pts',(-4.39453820875555,-18.9923914823906,
0.));
#10486=CARTESIAN_POINT('Ctrl Pts',(-4.39453820875555,-18.9923914823906,
21.));
#10487=CARTESIAN_POINT('Ctrl Pts',(-4.37168516143123,-18.9500107909187,
0.));
#10488=CARTESIAN_POINT('Ctrl Pts',(-4.37168516143123,-18.9500107909187,
21.));
#10489=CARTESIAN_POINT('Ctrl Pts',(-4.34926881342022,-18.9074876952706,
0.));
#10490=CARTESIAN_POINT('Ctrl Pts',(-4.34926881342022,-18.9074876952706,
21.));
#10491=CARTESIAN_POINT('Ctrl Pts',(-4.32737526247704,-18.8647973781745,
0.));
#10492=CARTESIAN_POINT('Ctrl Pts',(-4.32737526247704,-18.8647973781745,
21.));
#10493=CARTESIAN_POINT('Ctrl Pts',(-4.30608591031526,-18.8219166495975,
0.));
#10494=CARTESIAN_POINT('Ctrl Pts',(-4.30608591031526,-18.8219166495975,
21.));
#10495=CARTESIAN_POINT('Ctrl Pts',(-4.28545098663153,-18.778832216358,0.));
#10496=CARTESIAN_POINT('Ctrl Pts',(-4.28545098663153,-18.778832216358,21.));
#10497=CARTESIAN_POINT('Ctrl Pts',(-4.26546636161933,-18.735547949685,0.));
#10498=CARTESIAN_POINT('Ctrl Pts',(-4.26546636161933,-18.735547949685,21.));
#10499=CARTESIAN_POINT('Ctrl Pts',(-4.24603817988453,-18.6920958920047,
0.));
#10500=CARTESIAN_POINT('Ctrl Pts',(-4.24603817988453,-18.6920958920047,
21.));
#10501=CARTESIAN_POINT('Ctrl Pts',(-4.22703266508919,-18.6485210883348,
0.));
#10502=CARTESIAN_POINT('Ctrl Pts',(-4.22703266508919,-18.6485210883348,
21.));
#10503=CARTESIAN_POINT('Ctrl Pts',(-4.20834600700665,-18.6048602364653,
0.));
#10504=CARTESIAN_POINT('Ctrl Pts',(-4.20834600700665,-18.6048602364653,
21.));
#10505=CARTESIAN_POINT('Ctrl Pts',(-4.18996967278621,-18.5611217636409,
0.));
#10506=CARTESIAN_POINT('Ctrl Pts',(-4.18996967278621,-18.5611217636409,
21.));
#10507=CARTESIAN_POINT('Ctrl Pts',(-4.17205262766562,-18.5172668097744,
0.));
#10508=CARTESIAN_POINT('Ctrl Pts',(-4.17205262766562,-18.5172668097744,
21.));
#10509=CARTESIAN_POINT('Ctrl Pts',(-4.15497867673974,-18.4731856794913,
0.));
#10510=CARTESIAN_POINT('Ctrl Pts',(-4.15497867673974,-18.4731856794913,
21.));
#10511=CARTESIAN_POINT('Ctrl Pts',(-4.13926275457062,-18.4287286547442,
0.));
#10512=CARTESIAN_POINT('Ctrl Pts',(-4.13926275457062,-18.4287286547442,
21.));
#10513=CARTESIAN_POINT('Ctrl Pts',(-4.12819301671079,-18.3927403741815,
0.));
#10514=CARTESIAN_POINT('Ctrl Pts',(-4.12819301671079,-18.3927403741815,
21.));
#10515=CARTESIAN_POINT('Ctrl Pts',(-4.1209201986886,-18.3654573320481,0.));
#10516=CARTESIAN_POINT('Ctrl Pts',(-4.1209201986886,-18.3654573320481,21.));
#10517=CARTESIAN_POINT('Ctrl Pts',(-4.11655269114952,-18.3471320125699,
0.));
#10518=CARTESIAN_POINT('Ctrl Pts',(-4.11655269114952,-18.3471320125699,
21.));
#10519=CARTESIAN_POINT('Ctrl Pts',(-4.11448919812531,-18.337935196262,0.));
#10520=CARTESIAN_POINT('Ctrl Pts',(-4.11448919812531,-18.337935196262,21.));
#10521=CARTESIAN_POINT('',(-6.13422273260085,-21.1275013067528,0.));
#10522=CARTESIAN_POINT('Ctrl Pts',(-4.11448919812531,-18.337935196262,0.));
#10523=CARTESIAN_POINT('Ctrl Pts',(-4.11655269114952,-18.3471320125699,
0.));
#10524=CARTESIAN_POINT('Ctrl Pts',(-4.1209201986886,-18.3654573320481,0.));
#10525=CARTESIAN_POINT('Ctrl Pts',(-4.12819301671079,-18.3927403741815,
0.));
#10526=CARTESIAN_POINT('Ctrl Pts',(-4.13926275457062,-18.4287286547442,
0.));
#10527=CARTESIAN_POINT('Ctrl Pts',(-4.15497867673974,-18.4731856794913,
0.));
#10528=CARTESIAN_POINT('Ctrl Pts',(-4.17205262766562,-18.5172668097744,
0.));
#10529=CARTESIAN_POINT('Ctrl Pts',(-4.18996967278621,-18.5611217636409,
0.));
#10530=CARTESIAN_POINT('Ctrl Pts',(-4.20834600700665,-18.6048602364653,
0.));
#10531=CARTESIAN_POINT('Ctrl Pts',(-4.22703266508919,-18.6485210883348,
0.));
#10532=CARTESIAN_POINT('Ctrl Pts',(-4.24603817988453,-18.6920958920047,
0.));
#10533=CARTESIAN_POINT('Ctrl Pts',(-4.26546636161933,-18.735547949685,0.));
#10534=CARTESIAN_POINT('Ctrl Pts',(-4.28545098663153,-18.778832216358,0.));
#10535=CARTESIAN_POINT('Ctrl Pts',(-4.30608591031526,-18.8219166495975,
0.));
#10536=CARTESIAN_POINT('Ctrl Pts',(-4.32737526247704,-18.8647973781745,
0.));
#10537=CARTESIAN_POINT('Ctrl Pts',(-4.34926881342022,-18.9074876952706,
0.));
#10538=CARTESIAN_POINT('Ctrl Pts',(-4.37168516143123,-18.9500107909187,
0.));
#10539=CARTESIAN_POINT('Ctrl Pts',(-4.39453820875555,-18.9923914823906,
0.));
#10540=CARTESIAN_POINT('Ctrl Pts',(-4.41776558033332,-19.034647328575,0.));
#10541=CARTESIAN_POINT('Ctrl Pts',(-4.44134542994082,-19.0767833717249,
0.));
#10542=CARTESIAN_POINT('Ctrl Pts',(-4.46528051067022,-19.1187970904932,
0.));
#10543=CARTESIAN_POINT('Ctrl Pts',(-4.48958819710577,-19.1606814968494,
0.));
#10544=CARTESIAN_POINT('Ctrl Pts',(-4.51428889122955,-19.2024287376926,
0.));
#10545=CARTESIAN_POINT('Ctrl Pts',(-4.53939338835152,-19.2440340196551,
0.));
#10546=CARTESIAN_POINT('Ctrl Pts',(-4.56489651606741,-19.2854975819105,
0.));
#10547=CARTESIAN_POINT('Ctrl Pts',(-4.59078395765677,-19.3268225655679,
0.));
#10548=CARTESIAN_POINT('Ctrl Pts',(-4.61703633725712,-19.3680137353983,
0.));
#10549=CARTESIAN_POINT('Ctrl Pts',(-4.64363405547472,-19.4090759683639,
0.));
#10550=CARTESIAN_POINT('Ctrl Pts',(-4.67056260851454,-19.4500125912299,
0.));
#10551=CARTESIAN_POINT('Ctrl Pts',(-4.69781487613785,-19.4908246636763,
0.));
#10552=CARTESIAN_POINT('Ctrl Pts',(-4.72538815796616,-19.531511899192,0.));
#10553=CARTESIAN_POINT('Ctrl Pts',(-4.75328238194611,-19.5720732205813,
0.));
#10554=CARTESIAN_POINT('Ctrl Pts',(-4.78149799361731,-19.6125074152527,
0.));
#10555=CARTESIAN_POINT('Ctrl Pts',(-4.81003361418061,-19.6528138625329,
0.));
#10556=CARTESIAN_POINT('Ctrl Pts',(-4.83888510708974,-19.6929928227072,
0.));
#10557=CARTESIAN_POINT('Ctrl Pts',(-4.86804682289087,-19.7330450480715,
0.));
#10558=CARTESIAN_POINT('Ctrl Pts',(-4.89751233527805,-19.772971552601,0.));
#10559=CARTESIAN_POINT('Ctrl Pts',(-4.92727531494347,-19.8127733387903,
0.));
#10560=CARTESIAN_POINT('Ctrl Pts',(-4.95733049830096,-19.8524510953961,
0.));
#10561=CARTESIAN_POINT('Ctrl Pts',(-4.98767405031333,-19.8920050831202,
0.));
#10562=CARTESIAN_POINT('Ctrl Pts',(-5.01830302225558,-19.931435301086,0.));
#10563=CARTESIAN_POINT('Ctrl Pts',(-5.04921502064063,-19.9707415879783,
0.));
#10564=CARTESIAN_POINT('Ctrl Pts',(-5.08040781745337,-20.0099237417205,
0.));
#10565=CARTESIAN_POINT('Ctrl Pts',(-5.11187891582335,-20.0489816528155,
0.));
#10566=CARTESIAN_POINT('Ctrl Pts',(-5.14362537555398,-20.087915358486,0.));
#10567=CARTESIAN_POINT('Ctrl Pts',(-5.17564404279922,-20.1267249732337,
0.));
#10568=CARTESIAN_POINT('Ctrl Pts',(-5.20793168386164,-20.1654106491899,
0.));
#10569=CARTESIAN_POINT('Ctrl Pts',(-5.24048514441891,-20.2039725283917,
0.));
#10570=CARTESIAN_POINT('Ctrl Pts',(-5.27330152298151,-20.2424106921768,
0.));
#10571=CARTESIAN_POINT('Ctrl Pts',(-5.30637824220998,-20.2807251380077,
0.));
#10572=CARTESIAN_POINT('Ctrl Pts',(-5.33971294212214,-20.3189158047642,
0.));
#10573=CARTESIAN_POINT('Ctrl Pts',(-5.37330341114649,-20.3569825877537,
0.));
#10574=CARTESIAN_POINT('Ctrl Pts',(-5.40714750595875,-20.3949253578015,
0.));
#10575=CARTESIAN_POINT('Ctrl Pts',(-5.44124306065111,-20.4327439816542,
0.));
#10576=CARTESIAN_POINT('Ctrl Pts',(-5.47558784449851,-20.4704383353718,
0.));
#10577=CARTESIAN_POINT('Ctrl Pts',(-5.51017962306782,-20.5080083009242,
0.));
#10578=CARTESIAN_POINT('Ctrl Pts',(-5.5450161968946,-20.5454537676144,0.));
#10579=CARTESIAN_POINT('Ctrl Pts',(-5.58009544402475,-20.5827746317185,
0.));
#10580=CARTESIAN_POINT('Ctrl Pts',(-5.6154153671515,-20.6199707996366,0.));
#10581=CARTESIAN_POINT('Ctrl Pts',(-5.65097411164335,-20.6570421847033,
0.));
#10582=CARTESIAN_POINT('Ctrl Pts',(-5.68676990500164,-20.6939886877061,
0.));
#10583=CARTESIAN_POINT('Ctrl Pts',(-5.72280100798241,-20.7308101804425,
0.));
#10584=CARTESIAN_POINT('Ctrl Pts',(-5.75906566327796,-20.7675064905026,
0.));
#10585=CARTESIAN_POINT('Ctrl Pts',(-5.79556203439644,-20.8040773827343,
0.));
#10586=CARTESIAN_POINT('Ctrl Pts',(-5.83228817460178,-20.8405225541277,
0.));
#10587=CARTESIAN_POINT('Ctrl Pts',(-5.86924212736288,-20.8768416821402,
0.));
#10588=CARTESIAN_POINT('Ctrl Pts',(-5.906422006626,-20.9130344665641,0.));
#10589=CARTESIAN_POINT('Ctrl Pts',(-5.94382608200804,-20.9491006734021,
0.));
#10590=CARTESIAN_POINT('Ctrl Pts',(-5.98145286361837,-20.9850401822713,
0.));
#10591=CARTESIAN_POINT('Ctrl Pts',(-6.02687083887287,-21.0280155918661,
0.));
#10592=CARTESIAN_POINT('Ctrl Pts',(-6.06499496148845,-21.0636702474951,
0.));
#10593=CARTESIAN_POINT('Ctrl Pts',(-6.09567013127872,-21.0920928984154,
0.));
#10594=CARTESIAN_POINT('Ctrl Pts',(-6.11877533761501,-21.1133530893457,
0.));
#10595=CARTESIAN_POINT('Ctrl Pts',(-6.13422273260091,-21.1275013067528,
0.));
#10596=CARTESIAN_POINT('',(-6.13422273260085,-21.1275013067528,13.));
#10597=CARTESIAN_POINT('Ctrl Pts',(-6.13422273260091,-21.1275013067528,
13.));
#10598=CARTESIAN_POINT('Ctrl Pts',(-6.05818207473574,-21.0578559224639,
13.));
#10599=CARTESIAN_POINT('Ctrl Pts',(-5.98341417184727,-20.9874765040291,
13.));
#10600=CARTESIAN_POINT('Ctrl Pts',(-5.90994468705572,-20.91635991547,13.));
#10601=CARTESIAN_POINT('Ctrl Pts',(-5.78820256793373,-20.7985166473367,
13.));
#10602=CARTESIAN_POINT('Ctrl Pts',(-5.67003811891004,-20.6786545089329,
13.));
#10603=CARTESIAN_POINT('Ctrl Pts',(-5.55573863837939,-20.5568062999927,
13.));
#10604=CARTESIAN_POINT('Ctrl Pts',(-5.46788135574845,-20.4631466220902,
13.));
#10605=CARTESIAN_POINT('Ctrl Pts',(-5.38230707224949,-20.3683108766313,
13.));
#10606=CARTESIAN_POINT('Ctrl Pts',(-5.29917141503086,-20.272307558011,13.));
#10607=CARTESIAN_POINT('Ctrl Pts',(-5.20967788549041,-20.1689623013743,
13.));
#10608=CARTESIAN_POINT('Ctrl Pts',(-5.12300396000483,-20.0642651120126,
13.));
#10609=CARTESIAN_POINT('Ctrl Pts',(-5.03941267542058,-19.9582092065757,
13.));
#10610=CARTESIAN_POINT('Ctrl Pts',(-4.99313426716769,-19.8994937733358,
13.));
#10611=CARTESIAN_POINT('Ctrl Pts',(-4.9477958395688,-19.8403635603379,13.));
#10612=CARTESIAN_POINT('Ctrl Pts',(-4.90344584463339,-19.780817320786,13.));
#10613=CARTESIAN_POINT('Ctrl Pts',(-4.86070845370395,-19.72343623378,13.));
#10614=CARTESIAN_POINT('Ctrl Pts',(-4.81889538674849,-19.665666793385,13.));
#10615=CARTESIAN_POINT('Ctrl Pts',(-4.7780829655059,-19.607498635726,13.));
#10616=CARTESIAN_POINT('Ctrl Pts',(-4.74280851477666,-19.5572235050457,
13.));
#10617=CARTESIAN_POINT('Ctrl Pts',(-4.70827845306304,-19.5066514991033,
13.));
#10618=CARTESIAN_POINT('Ctrl Pts',(-4.67449772148844,-19.4557905173051,
13.));
#10619=CARTESIAN_POINT('Ctrl Pts',(-4.65025481897416,-19.4192898920658,
13.));
#10620=CARTESIAN_POINT('Ctrl Pts',(-4.62639514838843,-19.382641288743,13.));
#10621=CARTESIAN_POINT('Ctrl Pts',(-4.60295743063937,-19.3458364383459,
13.));
#10622=CARTESIAN_POINT('Ctrl Pts',(-4.57990136645455,-19.309630908347,13.));
#10623=CARTESIAN_POINT('Ctrl Pts',(-4.55725971984417,-19.273272273525,13.));
#10624=CARTESIAN_POINT('Ctrl Pts',(-4.5350835755811,-19.2367485575731,13.));
#10625=CARTESIAN_POINT('Ctrl Pts',(-4.51585555580649,-19.2050803503215,
13.));
#10626=CARTESIAN_POINT('Ctrl Pts',(-4.49697986255775,-19.1732873013029,
13.));
#10627=CARTESIAN_POINT('Ctrl Pts',(-4.47844262265296,-19.1413765621579,
13.));
#10628=CARTESIAN_POINT('Ctrl Pts',(-4.46165213670422,-19.1124727544724,
13.));
#10629=CARTESIAN_POINT('Ctrl Pts',(-4.4451340112905,-19.0834740456903,13.));
#10630=CARTESIAN_POINT('Ctrl Pts',(-4.42886646472448,-19.0543895552964,
13.));
#10631=CARTESIAN_POINT('Ctrl Pts',(-4.41516354268672,-19.0298903167199,
13.));
#10632=CARTESIAN_POINT('Ctrl Pts',(-4.40163676089501,-19.0053307306813,
13.));
#10633=CARTESIAN_POINT('Ctrl Pts',(-4.38830551710826,-18.9807063064772,
13.));
#10634=CARTESIAN_POINT('Ctrl Pts',(-4.36901375649227,-18.9450720847457,
13.));
#10635=CARTESIAN_POINT('Ctrl Pts',(-4.35013223002823,-18.9093017976319,
13.));
#10636=CARTESIAN_POINT('Ctrl Pts',(-4.33187128669082,-18.8733353264261,
13.));
#10637=CARTESIAN_POINT('Ctrl Pts',(-4.32083731653844,-18.8516029896876,
13.));
#10638=CARTESIAN_POINT('Ctrl Pts',(-4.31003325584325,-18.829798004179,13.));
#10639=CARTESIAN_POINT('Ctrl Pts',(-4.29948469303248,-18.807913802916,13.));
#10640=CARTESIAN_POINT('Ctrl Pts',(-4.28975595059153,-18.787730412872,13.));
#10641=CARTESIAN_POINT('Ctrl Pts',(-4.28024580001115,-18.7674792481688,
13.));
#10642=CARTESIAN_POINT('Ctrl Pts',(-4.27093067976999,-18.7471689057697,
13.));
#10643=CARTESIAN_POINT('Ctrl Pts',(-4.25811678809167,-18.7192299720025,
13.));
#10644=CARTESIAN_POINT('Ctrl Pts',(-4.24566493398932,-18.6911811213678,
13.));
#10645=CARTESIAN_POINT('Ctrl Pts',(-4.23343245343576,-18.6630711735883,
13.));
#10646=CARTESIAN_POINT('Ctrl Pts',(-4.22567194943,-18.6452377209709,13.));
#10647=CARTESIAN_POINT('Ctrl Pts',(-4.21799814921869,-18.6273802008519,
13.));
#10648=CARTESIAN_POINT('Ctrl Pts',(-4.21040342108815,-18.6095026819575,
13.));
#10649=CARTESIAN_POINT('Ctrl Pts',(-4.2035875060976,-18.5934584408824,13.));
#10650=CARTESIAN_POINT('Ctrl Pts',(-4.1968345819819,-18.5773983085029,13.));
#10651=CARTESIAN_POINT('Ctrl Pts',(-4.19017810368168,-18.5613135378487,
13.));
#10652=CARTESIAN_POINT('Ctrl Pts',(-4.18318081927935,-18.5444052404372,
13.));
#10653=CARTESIAN_POINT('Ctrl Pts',(-4.17628995976621,-18.5274697699669,
13.));
#10654=CARTESIAN_POINT('Ctrl Pts',(-4.16960404102653,-18.5104789585687,
13.));
#10655=CARTESIAN_POINT('Ctrl Pts',(-4.15849874475977,-18.4822572583451,
13.));
#10656=CARTESIAN_POINT('Ctrl Pts',(-4.14796697295268,-18.4538805850219,
13.));
#10657=CARTESIAN_POINT('Ctrl Pts',(-4.13860964460765,-18.4251735640106,
13.));
#10658=CARTESIAN_POINT('Ctrl Pts',(-4.13344968074392,-18.4093434909821,
13.));
#10659=CARTESIAN_POINT('Ctrl Pts',(-4.12864814562055,-18.3934125378936,
13.));
#10660=CARTESIAN_POINT('Ctrl Pts',(-4.1242788981144,-18.3773590065616,13.));
#10661=CARTESIAN_POINT('Ctrl Pts',(-4.1207247406093,-18.3643002867737,13.));
#10662=CARTESIAN_POINT('Ctrl Pts',(-4.11745655843684,-18.3511604736845,
13.));
#10663=CARTESIAN_POINT('Ctrl Pts',(-4.11448919812531,-18.337935196262,13.));
#10664=CARTESIAN_POINT('',(-6.13422273260085,-21.1275013067528,0.));
#10665=CARTESIAN_POINT('Origin',(-1.75106900012182E-12,-5.38923623413286E-12,
0.));
#10666=CARTESIAN_POINT('',(-7.45574324794401,-20.698113262342,0.));
#10667=CARTESIAN_POINT('Origin',(-1.75106900012182E-12,-5.38923623413286E-12,
0.));
#10668=CARTESIAN_POINT('',(-7.45574324794401,-20.698113262342,13.));
#10669=CARTESIAN_POINT('Origin',(-1.75106900012182E-12,-5.38923623413286E-12,
13.));
#10670=CARTESIAN_POINT('',(-7.45574324794401,-20.698113262342,0.));
#10671=CARTESIAN_POINT('Ctrl Pts',(-7.45007618140239,-17.2541372868972,
0.));
#10672=CARTESIAN_POINT('Ctrl Pts',(-7.45007618140239,-17.2541372868972,
21.));
#10673=CARTESIAN_POINT('Ctrl Pts',(-7.45381253347183,-17.2627905583523,
0.));
#10674=CARTESIAN_POINT('Ctrl Pts',(-7.45381253347183,-17.2627905583523,
21.));
#10675=CARTESIAN_POINT('Ctrl Pts',(-7.46105049818251,-17.2801832097582,
0.));
#10676=CARTESIAN_POINT('Ctrl Pts',(-7.46105049818251,-17.2801832097582,
21.));
#10677=CARTESIAN_POINT('Ctrl Pts',(-7.4712032346092,-17.3065305096784,0.));
#10678=CARTESIAN_POINT('Ctrl Pts',(-7.4712032346092,-17.3065305096784,21.));
#10679=CARTESIAN_POINT('Ctrl Pts',(-7.48340100912745,-17.3421522689127,
0.));
#10680=CARTESIAN_POINT('Ctrl Pts',(-7.48340100912745,-17.3421522689127,
21.));
#10681=CARTESIAN_POINT('Ctrl Pts',(-7.49681774451751,-17.3873563447297,
0.));
#10682=CARTESIAN_POINT('Ctrl Pts',(-7.49681774451751,-17.3873563447297,
21.));
#10683=CARTESIAN_POINT('Ctrl Pts',(-7.50891486634214,-17.4330545448126,
0.));
#10684=CARTESIAN_POINT('Ctrl Pts',(-7.50891486634214,-17.4330545448126,
21.));
#10685=CARTESIAN_POINT('Ctrl Pts',(-7.52019696747329,-17.4790653226646,
0.));
#10686=CARTESIAN_POINT('Ctrl Pts',(-7.52019696747329,-17.4790653226646,
21.));
#10687=CARTESIAN_POINT('Ctrl Pts',(-7.53103903007864,-17.5252518287336,
0.));
#10688=CARTESIAN_POINT('Ctrl Pts',(-7.53103903007864,-17.5252518287336,
21.));
#10689=CARTESIAN_POINT('Ctrl Pts',(-7.54158441095318,-17.5715579419204,
0.));
#10690=CARTESIAN_POINT('Ctrl Pts',(-7.54158441095318,-17.5715579419204,
21.));
#10691=CARTESIAN_POINT('Ctrl Pts',(-7.55182125346564,-17.6179818599248,
0.));
#10692=CARTESIAN_POINT('Ctrl Pts',(-7.55182125346564,-17.6179818599248,
21.));
#10693=CARTESIAN_POINT('Ctrl Pts',(-7.56164400295863,-17.6645549117314,
0.));
#10694=CARTESIAN_POINT('Ctrl Pts',(-7.56164400295863,-17.6645549117314,
21.));
#10695=CARTESIAN_POINT('Ctrl Pts',(-7.57091795530424,-17.7113192869136,
0.));
#10696=CARTESIAN_POINT('Ctrl Pts',(-7.57091795530424,-17.7113192869136,
21.));
#10697=CARTESIAN_POINT('Ctrl Pts',(-7.57954834582804,-17.7583042294209,
0.));
#10698=CARTESIAN_POINT('Ctrl Pts',(-7.57954834582804,-17.7583042294209,
21.));
#10699=CARTESIAN_POINT('Ctrl Pts',(-7.58752955799499,-17.8055090348024,
0.));
#10700=CARTESIAN_POINT('Ctrl Pts',(-7.58752955799499,-17.8055090348024,
21.));
#10701=CARTESIAN_POINT('Ctrl Pts',(-7.59491004201956,-17.8529149331931,
0.));
#10702=CARTESIAN_POINT('Ctrl Pts',(-7.59491004201956,-17.8529149331931,
21.));
#10703=CARTESIAN_POINT('Ctrl Pts',(-7.60176928403059,-17.900492838997,0.));
#10704=CARTESIAN_POINT('Ctrl Pts',(-7.60176928403059,-17.900492838997,21.));
#10705=CARTESIAN_POINT('Ctrl Pts',(-7.60819152580111,-17.9482122228183,
0.));
#10706=CARTESIAN_POINT('Ctrl Pts',(-7.60819152580111,-17.9482122228183,
21.));
#10707=CARTESIAN_POINT('Ctrl Pts',(-7.61423755067038,-17.9960506269561,
0.));
#10708=CARTESIAN_POINT('Ctrl Pts',(-7.61423755067038,-17.9960506269561,
21.));
#10709=CARTESIAN_POINT('Ctrl Pts',(-7.61992799636654,-18.0439992897906,
0.));
#10710=CARTESIAN_POINT('Ctrl Pts',(-7.61992799636654,-18.0439992897906,
21.));
#10711=CARTESIAN_POINT('Ctrl Pts',(-7.62525915358074,-18.0920577897363,
0.));
#10712=CARTESIAN_POINT('Ctrl Pts',(-7.62525915358074,-18.0920577897363,
21.));
#10713=CARTESIAN_POINT('Ctrl Pts',(-7.63021285851762,-18.1402306858819,
0.));
#10714=CARTESIAN_POINT('Ctrl Pts',(-7.63021285851762,-18.1402306858819,
21.));
#10715=CARTESIAN_POINT('Ctrl Pts',(-7.63476798969017,-18.1885236169197,
0.));
#10716=CARTESIAN_POINT('Ctrl Pts',(-7.63476798969017,-18.1885236169197,
21.));
#10717=CARTESIAN_POINT('Ctrl Pts',(-7.63891299603827,-18.2369390502576,
0.));
#10718=CARTESIAN_POINT('Ctrl Pts',(-7.63891299603827,-18.2369390502576,
21.));
#10719=CARTESIAN_POINT('Ctrl Pts',(-7.6426522027076,-18.2854741391282,0.));
#10720=CARTESIAN_POINT('Ctrl Pts',(-7.6426522027076,-18.2854741391282,21.));
#10721=CARTESIAN_POINT('Ctrl Pts',(-7.64599903846601,-18.3341230095852,
0.));
#10722=CARTESIAN_POINT('Ctrl Pts',(-7.64599903846601,-18.3341230095852,
21.));
#10723=CARTESIAN_POINT('Ctrl Pts',(-7.6489719793775,-18.3828781275628,0.));
#10724=CARTESIAN_POINT('Ctrl Pts',(-7.6489719793775,-18.3828781275628,21.));
#10725=CARTESIAN_POINT('Ctrl Pts',(-7.65158974829127,-18.4317319183719,
0.));
#10726=CARTESIAN_POINT('Ctrl Pts',(-7.65158974829127,-18.4317319183719,
21.));
#10727=CARTESIAN_POINT('Ctrl Pts',(-7.65386603444743,-18.4806785483052,
0.));
#10728=CARTESIAN_POINT('Ctrl Pts',(-7.65386603444743,-18.4806785483052,
21.));
#10729=CARTESIAN_POINT('Ctrl Pts',(-7.65580722110437,-18.5297146894905,
0.));
#10730=CARTESIAN_POINT('Ctrl Pts',(-7.65580722110437,-18.5297146894905,
21.));
#10731=CARTESIAN_POINT('Ctrl Pts',(-7.65741532450727,-18.5788385228928,
0.));
#10732=CARTESIAN_POINT('Ctrl Pts',(-7.65741532450727,-18.5788385228928,
21.));
#10733=CARTESIAN_POINT('Ctrl Pts',(-7.65868976978872,-18.6280491346907,
0.));
#10734=CARTESIAN_POINT('Ctrl Pts',(-7.65868976978872,-18.6280491346907,
21.));
#10735=CARTESIAN_POINT('Ctrl Pts',(-7.65962948375622,-18.6773458057584,
0.));
#10736=CARTESIAN_POINT('Ctrl Pts',(-7.65962948375622,-18.6773458057584,
21.));
#10737=CARTESIAN_POINT('Ctrl Pts',(-7.66023521705905,-18.7267272235231,
0.));
#10738=CARTESIAN_POINT('Ctrl Pts',(-7.66023521705905,-18.7267272235231,
21.));
#10739=CARTESIAN_POINT('Ctrl Pts',(-7.66051046922541,-18.7761911671591,
0.));
#10740=CARTESIAN_POINT('Ctrl Pts',(-7.66051046922541,-18.7761911671591,
21.));
#10741=CARTESIAN_POINT('Ctrl Pts',(-7.66046025294775,-18.8257349246207,
0.));
#10742=CARTESIAN_POINT('Ctrl Pts',(-7.66046025294775,-18.8257349246207,
21.));
#10743=CARTESIAN_POINT('Ctrl Pts',(-7.66009036321663,-18.8753555389435,
0.));
#10744=CARTESIAN_POINT('Ctrl Pts',(-7.66009036321663,-18.8753555389435,
21.));
#10745=CARTESIAN_POINT('Ctrl Pts',(-7.65940650980099,-18.9250501008887,
0.));
#10746=CARTESIAN_POINT('Ctrl Pts',(-7.65940650980099,-18.9250501008887,
21.));
#10747=CARTESIAN_POINT('Ctrl Pts',(-7.65841335587266,-18.974816073814,0.));
#10748=CARTESIAN_POINT('Ctrl Pts',(-7.65841335587266,-18.974816073814,21.));
#10749=CARTESIAN_POINT('Ctrl Pts',(-7.65711415727855,-19.0246514144531,
0.));
#10750=CARTESIAN_POINT('Ctrl Pts',(-7.65711415727855,-19.0246514144531,
21.));
#10751=CARTESIAN_POINT('Ctrl Pts',(-7.65551129907202,-19.0745543888799,
0.));
#10752=CARTESIAN_POINT('Ctrl Pts',(-7.65551129907202,-19.0745543888799,
21.));
#10753=CARTESIAN_POINT('Ctrl Pts',(-7.65360662280609,-19.1245234597312,
0.));
#10754=CARTESIAN_POINT('Ctrl Pts',(-7.65360662280609,-19.1245234597312,
21.));
#10755=CARTESIAN_POINT('Ctrl Pts',(-7.65140181220526,-19.1745571539291,
0.));
#10756=CARTESIAN_POINT('Ctrl Pts',(-7.65140181220526,-19.1745571539291,
21.));
#10757=CARTESIAN_POINT('Ctrl Pts',(-7.64889882291924,-19.224653915265,0.));
#10758=CARTESIAN_POINT('Ctrl Pts',(-7.64889882291924,-19.224653915265,21.));
#10759=CARTESIAN_POINT('Ctrl Pts',(-7.64610005549614,-19.2748120456486,
0.));
#10760=CARTESIAN_POINT('Ctrl Pts',(-7.64610005549614,-19.2748120456486,
21.));
#10761=CARTESIAN_POINT('Ctrl Pts',(-7.64300812875339,-19.3250297839295,
0.));
#10762=CARTESIAN_POINT('Ctrl Pts',(-7.64300812875339,-19.3250297839295,
21.));
#10763=CARTESIAN_POINT('Ctrl Pts',(-7.63962574822761,-19.3753053524647,
0.));
#10764=CARTESIAN_POINT('Ctrl Pts',(-7.63962574822761,-19.3753053524647,
21.));
#10765=CARTESIAN_POINT('Ctrl Pts',(-7.63595554930654,-19.4256370121006,
0.));
#10766=CARTESIAN_POINT('Ctrl Pts',(-7.63595554930654,-19.4256370121006,
21.));
#10767=CARTESIAN_POINT('Ctrl Pts',(-7.63199992715366,-19.4760231231881,
0.));
#10768=CARTESIAN_POINT('Ctrl Pts',(-7.63199992715366,-19.4760231231881,
21.));
#10769=CARTESIAN_POINT('Ctrl Pts',(-7.62776096538883,-19.5264621687521,
0.));
#10770=CARTESIAN_POINT('Ctrl Pts',(-7.62776096538883,-19.5264621687521,
21.));
#10771=CARTESIAN_POINT('Ctrl Pts',(-7.6232405373522,-19.5769527121826,0.));
#10772=CARTESIAN_POINT('Ctrl Pts',(-7.6232405373522,-19.5769527121826,21.));
#10773=CARTESIAN_POINT('Ctrl Pts',(-7.61844037070591,-19.6274933688524,
0.));
#10774=CARTESIAN_POINT('Ctrl Pts',(-7.61844037070591,-19.6274933688524,
21.));
#10775=CARTESIAN_POINT('Ctrl Pts',(-7.61336212350879,-19.6780827744426,
0.));
#10776=CARTESIAN_POINT('Ctrl Pts',(-7.61336212350879,-19.6780827744426,
21.));
#10777=CARTESIAN_POINT('Ctrl Pts',(-7.60800746969262,-19.7287195480601,
0.));
#10778=CARTESIAN_POINT('Ctrl Pts',(-7.60800746969262,-19.7287195480601,
21.));
#10779=CARTESIAN_POINT('Ctrl Pts',(-7.60237814110187,-19.7794022782484,
0.));
#10780=CARTESIAN_POINT('Ctrl Pts',(-7.60237814110187,-19.7794022782484,
21.));
#10781=CARTESIAN_POINT('Ctrl Pts',(-7.59647587605448,-19.830129556152,0.));
#10782=CARTESIAN_POINT('Ctrl Pts',(-7.59647587605448,-19.830129556152,21.));
#10783=CARTESIAN_POINT('Ctrl Pts',(-7.59030238888852,-19.8808999994024,
0.));
#10784=CARTESIAN_POINT('Ctrl Pts',(-7.59030238888852,-19.8808999994024,
21.));
#10785=CARTESIAN_POINT('Ctrl Pts',(-7.58385933533352,-19.931712276832,0.));
#10786=CARTESIAN_POINT('Ctrl Pts',(-7.58385933533352,-19.931712276832,21.));
#10787=CARTESIAN_POINT('Ctrl Pts',(-7.57714827622806,-19.9825651387294,
0.));
#10788=CARTESIAN_POINT('Ctrl Pts',(-7.57714827622806,-19.9825651387294,
21.));
#10789=CARTESIAN_POINT('Ctrl Pts',(-7.57017066105973,-20.0334574248556,
0.));
#10790=CARTESIAN_POINT('Ctrl Pts',(-7.57017066105973,-20.0334574248556,
21.));
#10791=CARTESIAN_POINT('Ctrl Pts',(-7.56292786549461,-20.0843880130978,
0.));
#10792=CARTESIAN_POINT('Ctrl Pts',(-7.56292786549461,-20.0843880130978,
21.));
#10793=CARTESIAN_POINT('Ctrl Pts',(-7.55542122125495,-20.1353557774357,
0.));
#10794=CARTESIAN_POINT('Ctrl Pts',(-7.55542122125495,-20.1353557774357,
21.));
#10795=CARTESIAN_POINT('Ctrl Pts',(-7.54765204869255,-20.1863595454674,
0.));
#10796=CARTESIAN_POINT('Ctrl Pts',(-7.54765204869255,-20.1863595454674,
21.));
#10797=CARTESIAN_POINT('Ctrl Pts',(-7.53962169534167,-20.2373980474879,
0.));
#10798=CARTESIAN_POINT('Ctrl Pts',(-7.53962169534167,-20.2373980474879,
21.));
#10799=CARTESIAN_POINT('Ctrl Pts',(-7.53133155804008,-20.2884698940944,
0.));
#10800=CARTESIAN_POINT('Ctrl Pts',(-7.53133155804008,-20.2884698940944,
21.));
#10801=CARTESIAN_POINT('Ctrl Pts',(-7.52278303006887,-20.3395736743243,
0.));
#10802=CARTESIAN_POINT('Ctrl Pts',(-7.52278303006887,-20.3395736743243,
21.));
#10803=CARTESIAN_POINT('Ctrl Pts',(-7.51397746081994,-20.3907080367098,
0.));
#10804=CARTESIAN_POINT('Ctrl Pts',(-7.51397746081994,-20.3907080367098,
21.));
#10805=CARTESIAN_POINT('Ctrl Pts',(-7.50491611266253,-20.4418717748497,
0.));
#10806=CARTESIAN_POINT('Ctrl Pts',(-7.50491611266253,-20.4418717748497,
21.));
#10807=CARTESIAN_POINT('Ctrl Pts',(-7.49560012018406,-20.493063915616,0.));
#10808=CARTESIAN_POINT('Ctrl Pts',(-7.49560012018406,-20.493063915616,21.));
#10809=CARTESIAN_POINT('Ctrl Pts',(-7.48603045196745,-20.5442837929044,
0.));
#10810=CARTESIAN_POINT('Ctrl Pts',(-7.48603045196745,-20.5442837929044,
21.));
#10811=CARTESIAN_POINT('Ctrl Pts',(-7.47620789245428,-20.5955309838521,
0.));
#10812=CARTESIAN_POINT('Ctrl Pts',(-7.47620789245428,-20.5955309838521,
21.));
#10813=CARTESIAN_POINT('Ctrl Pts',(-7.46814799701906,-20.6365504027501,
0.));
#10814=CARTESIAN_POINT('Ctrl Pts',(-7.46814799701906,-20.6365504027501,
21.));
#10815=CARTESIAN_POINT('Ctrl Pts',(-7.46198969876654,-20.6673271112931,
0.));
#10816=CARTESIAN_POINT('Ctrl Pts',(-7.46198969876654,-20.6673271112931,
21.));
#10817=CARTESIAN_POINT('Ctrl Pts',(-7.45783379370108,-20.6878503127065,
0.));
#10818=CARTESIAN_POINT('Ctrl Pts',(-7.45783379370108,-20.6878503127065,
21.));
#10819=CARTESIAN_POINT('Ctrl Pts',(-7.45574324794401,-20.698113262342,0.));
#10820=CARTESIAN_POINT('Ctrl Pts',(-7.45574324794401,-20.698113262342,21.));
#10821=CARTESIAN_POINT('Ctrl Pts',(-7.45007618140239,-17.2541372868972,
0.));
#10822=CARTESIAN_POINT('Ctrl Pts',(-7.45381253347183,-17.2627905583523,
0.));
#10823=CARTESIAN_POINT('Ctrl Pts',(-7.46105049818251,-17.2801832097582,
0.));
#10824=CARTESIAN_POINT('Ctrl Pts',(-7.4712032346092,-17.3065305096784,0.));
#10825=CARTESIAN_POINT('Ctrl Pts',(-7.48340100912745,-17.3421522689127,
0.));
#10826=CARTESIAN_POINT('Ctrl Pts',(-7.49681774451751,-17.3873563447297,
0.));
#10827=CARTESIAN_POINT('Ctrl Pts',(-7.50891486634214,-17.4330545448126,
0.));
#10828=CARTESIAN_POINT('Ctrl Pts',(-7.52019696747329,-17.4790653226646,
0.));
#10829=CARTESIAN_POINT('Ctrl Pts',(-7.53103903007864,-17.5252518287336,
0.));
#10830=CARTESIAN_POINT('Ctrl Pts',(-7.54158441095318,-17.5715579419204,
0.));
#10831=CARTESIAN_POINT('Ctrl Pts',(-7.55182125346564,-17.6179818599248,
0.));
#10832=CARTESIAN_POINT('Ctrl Pts',(-7.56164400295863,-17.6645549117314,
0.));
#10833=CARTESIAN_POINT('Ctrl Pts',(-7.57091795530424,-17.7113192869136,
0.));
#10834=CARTESIAN_POINT('Ctrl Pts',(-7.57954834582804,-17.7583042294209,
0.));
#10835=CARTESIAN_POINT('Ctrl Pts',(-7.58752955799499,-17.8055090348024,
0.));
#10836=CARTESIAN_POINT('Ctrl Pts',(-7.59491004201956,-17.8529149331931,
0.));
#10837=CARTESIAN_POINT('Ctrl Pts',(-7.60176928403059,-17.900492838997,0.));
#10838=CARTESIAN_POINT('Ctrl Pts',(-7.60819152580111,-17.9482122228183,
0.));
#10839=CARTESIAN_POINT('Ctrl Pts',(-7.61423755067038,-17.9960506269561,
0.));
#10840=CARTESIAN_POINT('Ctrl Pts',(-7.61992799636654,-18.0439992897906,
0.));
#10841=CARTESIAN_POINT('Ctrl Pts',(-7.62525915358074,-18.0920577897363,
0.));
#10842=CARTESIAN_POINT('Ctrl Pts',(-7.63021285851762,-18.1402306858819,
0.));
#10843=CARTESIAN_POINT('Ctrl Pts',(-7.63476798969017,-18.1885236169197,
0.));
#10844=CARTESIAN_POINT('Ctrl Pts',(-7.63891299603827,-18.2369390502576,
0.));
#10845=CARTESIAN_POINT('Ctrl Pts',(-7.6426522027076,-18.2854741391282,0.));
#10846=CARTESIAN_POINT('Ctrl Pts',(-7.64599903846601,-18.3341230095852,
0.));
#10847=CARTESIAN_POINT('Ctrl Pts',(-7.6489719793775,-18.3828781275628,0.));
#10848=CARTESIAN_POINT('Ctrl Pts',(-7.65158974829127,-18.4317319183719,
0.));
#10849=CARTESIAN_POINT('Ctrl Pts',(-7.65386603444743,-18.4806785483052,
0.));
#10850=CARTESIAN_POINT('Ctrl Pts',(-7.65580722110437,-18.5297146894905,
0.));
#10851=CARTESIAN_POINT('Ctrl Pts',(-7.65741532450727,-18.5788385228928,
0.));
#10852=CARTESIAN_POINT('Ctrl Pts',(-7.65868976978872,-18.6280491346907,
0.));
#10853=CARTESIAN_POINT('Ctrl Pts',(-7.65962948375622,-18.6773458057584,
0.));
#10854=CARTESIAN_POINT('Ctrl Pts',(-7.66023521705905,-18.7267272235231,
0.));
#10855=CARTESIAN_POINT('Ctrl Pts',(-7.66051046922541,-18.7761911671591,
0.));
#10856=CARTESIAN_POINT('Ctrl Pts',(-7.66046025294775,-18.8257349246207,
0.));
#10857=CARTESIAN_POINT('Ctrl Pts',(-7.66009036321663,-18.8753555389435,
0.));
#10858=CARTESIAN_POINT('Ctrl Pts',(-7.65940650980099,-18.9250501008887,
0.));
#10859=CARTESIAN_POINT('Ctrl Pts',(-7.65841335587266,-18.974816073814,0.));
#10860=CARTESIAN_POINT('Ctrl Pts',(-7.65711415727855,-19.0246514144531,
0.));
#10861=CARTESIAN_POINT('Ctrl Pts',(-7.65551129907202,-19.0745543888799,
0.));
#10862=CARTESIAN_POINT('Ctrl Pts',(-7.65360662280609,-19.1245234597312,
0.));
#10863=CARTESIAN_POINT('Ctrl Pts',(-7.65140181220526,-19.1745571539291,
0.));
#10864=CARTESIAN_POINT('Ctrl Pts',(-7.64889882291924,-19.224653915265,0.));
#10865=CARTESIAN_POINT('Ctrl Pts',(-7.64610005549614,-19.2748120456486,
0.));
#10866=CARTESIAN_POINT('Ctrl Pts',(-7.64300812875339,-19.3250297839295,
0.));
#10867=CARTESIAN_POINT('Ctrl Pts',(-7.63962574822761,-19.3753053524647,
0.));
#10868=CARTESIAN_POINT('Ctrl Pts',(-7.63595554930654,-19.4256370121006,
0.));
#10869=CARTESIAN_POINT('Ctrl Pts',(-7.63199992715366,-19.4760231231881,
0.));
#10870=CARTESIAN_POINT('Ctrl Pts',(-7.62776096538883,-19.5264621687521,
0.));
#10871=CARTESIAN_POINT('Ctrl Pts',(-7.6232405373522,-19.5769527121826,0.));
#10872=CARTESIAN_POINT('Ctrl Pts',(-7.61844037070591,-19.6274933688524,
0.));
#10873=CARTESIAN_POINT('Ctrl Pts',(-7.61336212350879,-19.6780827744426,
0.));
#10874=CARTESIAN_POINT('Ctrl Pts',(-7.60800746969262,-19.7287195480601,
0.));
#10875=CARTESIAN_POINT('Ctrl Pts',(-7.60237814110187,-19.7794022782484,
0.));
#10876=CARTESIAN_POINT('Ctrl Pts',(-7.59647587605448,-19.830129556152,0.));
#10877=CARTESIAN_POINT('Ctrl Pts',(-7.59030238888852,-19.8808999994024,
0.));
#10878=CARTESIAN_POINT('Ctrl Pts',(-7.58385933533352,-19.931712276832,0.));
#10879=CARTESIAN_POINT('Ctrl Pts',(-7.57714827622806,-19.9825651387294,
0.));
#10880=CARTESIAN_POINT('Ctrl Pts',(-7.57017066105973,-20.0334574248556,
0.));
#10881=CARTESIAN_POINT('Ctrl Pts',(-7.56292786549461,-20.0843880130978,
0.));
#10882=CARTESIAN_POINT('Ctrl Pts',(-7.55542122125495,-20.1353557774357,
0.));
#10883=CARTESIAN_POINT('Ctrl Pts',(-7.54765204869255,-20.1863595454674,
0.));
#10884=CARTESIAN_POINT('Ctrl Pts',(-7.53962169534167,-20.2373980474879,
0.));
#10885=CARTESIAN_POINT('Ctrl Pts',(-7.53133155804008,-20.2884698940944,
0.));
#10886=CARTESIAN_POINT('Ctrl Pts',(-7.52278303006887,-20.3395736743243,
0.));
#10887=CARTESIAN_POINT('Ctrl Pts',(-7.51397746081994,-20.3907080367098,
0.));
#10888=CARTESIAN_POINT('Ctrl Pts',(-7.50491611266253,-20.4418717748497,
0.));
#10889=CARTESIAN_POINT('Ctrl Pts',(-7.49560012018406,-20.493063915616,0.));
#10890=CARTESIAN_POINT('Ctrl Pts',(-7.48411651832413,-20.5545277683621,
0.));
#10891=CARTESIAN_POINT('Ctrl Pts',(-7.47423073598682,-20.6057817877246,
0.));
#10892=CARTESIAN_POINT('Ctrl Pts',(-7.46612041736314,-20.6468066077586,
0.));
#10893=CARTESIAN_POINT('Ctrl Pts',(-7.45992433946824,-20.6775873630604,
0.));
#10894=CARTESIAN_POINT('Ctrl Pts',(-7.45574324794401,-20.698113262342,0.));
#10895=CARTESIAN_POINT('Ctrl Pts',(-7.45007618140239,-17.2541372868972,
13.));
#10896=CARTESIAN_POINT('Ctrl Pts',(-7.45637364573816,-17.2687220121489,
13.));
#10897=CARTESIAN_POINT('Ctrl Pts',(-7.46226667103919,-17.2834550499008,
13.));
#10898=CARTESIAN_POINT('Ctrl Pts',(-7.46778231425445,-17.2983267669067,
13.));
#10899=CARTESIAN_POINT('Ctrl Pts',(-7.47424706065699,-17.3157575315993,
13.));
#10900=CARTESIAN_POINT('Ctrl Pts',(-7.48019417753821,-17.3333785326113,
13.));
#10901=CARTESIAN_POINT('Ctrl Pts',(-7.48573450280811,-17.3511502187375,
13.));
#10902=CARTESIAN_POINT('Ctrl Pts',(-7.49353000563121,-17.3761558316968,
13.));
#10903=CARTESIAN_POINT('Ctrl Pts',(-7.50052692940225,-17.4014574303076,
13.));
#10904=CARTESIAN_POINT('Ctrl Pts',(-7.50711117101491,-17.4269165094415,
13.));
#10905=CARTESIAN_POINT('Ctrl Pts',(-7.51149073008789,-17.4438508122163,
13.));
#10906=CARTESIAN_POINT('Ctrl Pts',(-7.51568961154288,-17.4608540901313,
13.));
#10907=CARTESIAN_POINT('Ctrl Pts',(-7.51979276933228,-17.477895354957,13.));
#10908=CARTESIAN_POINT('Ctrl Pts',(-7.52411201550939,-17.4958340796489,
13.));
#10909=CARTESIAN_POINT('Ctrl Pts',(-7.52832602172309,-17.5138146001159,
13.));
#10910=CARTESIAN_POINT('Ctrl Pts',(-7.53247314101538,-17.5318219263269,
13.));
#10911=CARTESIAN_POINT('Ctrl Pts',(-7.53707874400482,-17.5518200478141,
13.));
#10912=CARTESIAN_POINT('Ctrl Pts',(-7.54160061545737,-17.5718516505912,
13.));
#10913=CARTESIAN_POINT('Ctrl Pts',(-7.5460260137895,-17.5919190740356,13.));
#10914=CARTESIAN_POINT('Ctrl Pts',(-7.55269751656612,-17.6221716888696,
13.));
#10915=CARTESIAN_POINT('Ctrl Pts',(-7.55914375118857,-17.6525076946371,
13.));
#10916=CARTESIAN_POINT('Ctrl Pts',(-7.56521559976811,-17.6829731243219,
13.));
#10917=CARTESIAN_POINT('Ctrl Pts',(-7.56962666501585,-17.7051055929398,
13.));
#10918=CARTESIAN_POINT('Ctrl Pts',(-7.57383703867015,-17.727307481075,13.));
#10919=CARTESIAN_POINT('Ctrl Pts',(-7.57782678310872,-17.7495842479971,
13.));
#10920=CARTESIAN_POINT('Ctrl Pts',(-7.58270390405109,-17.7768156880447,
13.));
#10921=CARTESIAN_POINT('Ctrl Pts',(-7.58725254420668,-17.8041586050554,
13.));
#10922=CARTESIAN_POINT('Ctrl Pts',(-7.59151733245669,-17.8315958504975,
13.));
#10923=CARTESIAN_POINT('Ctrl Pts',(-7.59612401157578,-17.8612326292199,
13.));
#10924=CARTESIAN_POINT('Ctrl Pts',(-7.60040516926074,-17.890977551337,13.));
#10925=CARTESIAN_POINT('Ctrl Pts',(-7.60444696777948,-17.9207992272247,
13.));
#10926=CARTESIAN_POINT('Ctrl Pts',(-7.60817833718655,-17.9483304583238,
13.));
#10927=CARTESIAN_POINT('Ctrl Pts',(-7.61170808544497,-17.9759263070057,
13.));
#10928=CARTESIAN_POINT('Ctrl Pts',(-7.61506270604885,-18.0035762489904,
13.));
#10929=CARTESIAN_POINT('Ctrl Pts',(-7.61962013038026,-18.0411401148466,
13.));
#10930=CARTESIAN_POINT('Ctrl Pts',(-7.62385245909278,-18.078804438117,13.));
#10931=CARTESIAN_POINT('Ctrl Pts',(-7.62773031180414,-18.1165756810882,
13.));
#10932=CARTESIAN_POINT('Ctrl Pts',(-7.63147235591759,-18.1530241147805,
13.));
#10933=CARTESIAN_POINT('Ctrl Pts',(-7.63487692331431,-18.1895746220981,
13.));
#10934=CARTESIAN_POINT('Ctrl Pts',(-7.63792794642091,-18.226229844125,13.));
#10935=CARTESIAN_POINT('Ctrl Pts',(-7.6420728467942,-18.2760269902476,13.));
#10936=CARTESIAN_POINT('Ctrl Pts',(-7.64556831472346,-18.3260163399595,
13.));
#10937=CARTESIAN_POINT('Ctrl Pts',(-7.64849356609124,-18.3761647741053,
13.));
#10938=CARTESIAN_POINT('Ctrl Pts',(-7.65106479845333,-18.4202441575742,
13.));
#10939=CARTESIAN_POINT('Ctrl Pts',(-7.65320196597273,-18.4644442731323,
13.));
#10940=CARTESIAN_POINT('Ctrl Pts',(-7.65493429570881,-18.5087513218567,
13.));
#10941=CARTESIAN_POINT('Ctrl Pts',(-7.65748817031469,-18.5740706685388,
13.));
#10942=CARTESIAN_POINT('Ctrl Pts',(-7.65915358769517,-18.6396252901705,
13.));
#10943=CARTESIAN_POINT('Ctrl Pts',(-7.65993127489945,-18.7054034394317,
13.));
#10944=CARTESIAN_POINT('Ctrl Pts',(-7.66091272374024,-18.7884161056895,
13.));
#10945=CARTESIAN_POINT('Ctrl Pts',(-7.66048522719283,-18.8717830756661,
13.));
#10946=CARTESIAN_POINT('Ctrl Pts',(-7.65875983806947,-18.9554457129062,
13.));
#10947=CARTESIAN_POINT('Ctrl Pts',(-7.65642266547867,-19.0687732052289,
13.));
#10948=CARTESIAN_POINT('Ctrl Pts',(-7.65169843824266,-19.1826450748833,
13.));
#10949=CARTESIAN_POINT('Ctrl Pts',(-7.64469887386167,-19.2969757396511,
13.));
#10950=CARTESIAN_POINT('Ctrl Pts',(-7.63845857891806,-19.3989045212746,
13.));
#10951=CARTESIAN_POINT('Ctrl Pts',(-7.63041784747171,-19.5011952230427,
13.));
#10952=CARTESIAN_POINT('Ctrl Pts',(-7.62065725315813,-19.6037897795036,
13.));
#10953=CARTESIAN_POINT('Ctrl Pts',(-7.6068238069441,-19.7491944785472,13.));
#10954=CARTESIAN_POINT('Ctrl Pts',(-7.5895301524174,-19.8952104286167,13.));
#10955=CARTESIAN_POINT('Ctrl Pts',(-7.56895177464837,-20.0416957573265,
13.));
#10956=CARTESIAN_POINT('Ctrl Pts',(-7.55296697971251,-20.15548208037,13.));
#10957=CARTESIAN_POINT('Ctrl Pts',(-7.53499708076544,-20.2695554921735,
13.));
#10958=CARTESIAN_POINT('Ctrl Pts',(-7.51511029118453,-20.3838501740658,
13.));
#10959=CARTESIAN_POINT('Ctrl Pts',(-7.4979067159171,-20.482723707906,13.));
#10960=CARTESIAN_POINT('Ctrl Pts',(-7.47927116738907,-20.5817593863818,
13.));
#10961=CARTESIAN_POINT('Ctrl Pts',(-7.45922688157452,-20.6809436221336,
13.));
#10962=CARTESIAN_POINT('Ctrl Pts',(-7.45807037084351,-20.6866663320398,
13.));
#10963=CARTESIAN_POINT('Ctrl Pts',(-7.45690915954643,-20.6923895454539,
13.));
#10964=CARTESIAN_POINT('Ctrl Pts',(-7.45574324794401,-20.698113262342,13.));
#10965=CARTESIAN_POINT('Ctrl Pts',(-12.3627494547115,-18.1978687191668,
0.));
#10966=CARTESIAN_POINT('Ctrl Pts',(-12.3627494547115,-18.1978687191668,
21.));
#10967=CARTESIAN_POINT('Ctrl Pts',(-12.3532177620787,-18.1935275957711,
0.));
#10968=CARTESIAN_POINT('Ctrl Pts',(-12.3532177620787,-18.1935275957711,
21.));
#10969=CARTESIAN_POINT('Ctrl Pts',(-12.3341713636489,-18.1848265584754,
0.));
#10970=CARTESIAN_POINT('Ctrl Pts',(-12.3341713636489,-18.1848265584754,
21.));
#10971=CARTESIAN_POINT('Ctrl Pts',(-12.3056527265146,-18.1717186310224,
0.));
#10972=CARTESIAN_POINT('Ctrl Pts',(-12.3056527265146,-18.1717186310224,
21.));
#10973=CARTESIAN_POINT('Ctrl Pts',(-12.2677298318549,-18.1541286139166,
0.));
#10974=CARTESIAN_POINT('Ctrl Pts',(-12.2677298318549,-18.1541286139166,
21.));
#10975=CARTESIAN_POINT('Ctrl Pts',(-12.2204964278426,-18.1319528884305,
0.));
#10976=CARTESIAN_POINT('Ctrl Pts',(-12.2204964278426,-18.1319528884305,
21.));
#10977=CARTESIAN_POINT('Ctrl Pts',(-12.1734337668195,-18.109588624154,0.));
#10978=CARTESIAN_POINT('Ctrl Pts',(-12.1734337668195,-18.109588624154,21.));
#10979=CARTESIAN_POINT('Ctrl Pts',(-12.1265426519718,-18.0870354350128,
0.));
#10980=CARTESIAN_POINT('Ctrl Pts',(-12.1265426519718,-18.0870354350128,
21.));
#10981=CARTESIAN_POINT('Ctrl Pts',(-12.0798241915081,-18.0642929289333,
0.));
#10982=CARTESIAN_POINT('Ctrl Pts',(-12.0798241915081,-18.0642929289333,
21.));
#10983=CARTESIAN_POINT('Ctrl Pts',(-12.0332798395991,-18.0413607600052,
0.));
#10984=CARTESIAN_POINT('Ctrl Pts',(-12.0332798395991,-18.0413607600052,
21.));
#10985=CARTESIAN_POINT('Ctrl Pts',(-11.986911314246,-18.0182386160553,0.));
#10986=CARTESIAN_POINT('Ctrl Pts',(-11.986911314246,-18.0182386160553,21.));
#10987=CARTESIAN_POINT('Ctrl Pts',(-11.9407205019619,-17.9949261997754,
0.));
#10988=CARTESIAN_POINT('Ctrl Pts',(-11.9407205019619,-17.9949261997754,
21.));
#10989=CARTESIAN_POINT('Ctrl Pts',(-11.8947093631895,-17.9714232133203,
0.));
#10990=CARTESIAN_POINT('Ctrl Pts',(-11.8947093631895,-17.9714232133203,
21.));
#10991=CARTESIAN_POINT('Ctrl Pts',(-11.8488798430201,-17.9477293432951,
0.));
#10992=CARTESIAN_POINT('Ctrl Pts',(-11.8488798430201,-17.9477293432951,
21.));
#10993=CARTESIAN_POINT('Ctrl Pts',(-11.8032337607271,-17.9238442458356,
0.));
#10994=CARTESIAN_POINT('Ctrl Pts',(-11.8032337607271,-17.9238442458356,
21.));
#10995=CARTESIAN_POINT('Ctrl Pts',(-11.7577728408871,-17.8997675418752,
0.));
#10996=CARTESIAN_POINT('Ctrl Pts',(-11.7577728408871,-17.8997675418752,
21.));
#10997=CARTESIAN_POINT('Ctrl Pts',(-11.7124987772363,-17.8754988158862,
0.));
#10998=CARTESIAN_POINT('Ctrl Pts',(-11.7124987772363,-17.8754988158862,
21.));
#10999=CARTESIAN_POINT('Ctrl Pts',(-11.6674132861792,-17.8510376144926,
0.));
#11000=CARTESIAN_POINT('Ctrl Pts',(-11.6674132861792,-17.8510376144926,
21.));
#11001=CARTESIAN_POINT('Ctrl Pts',(-11.6225181583564,-17.8263834470057,
0.));
#11002=CARTESIAN_POINT('Ctrl Pts',(-11.6225181583564,-17.8263834470057,
21.));
#11003=CARTESIAN_POINT('Ctrl Pts',(-11.5778153222435,-17.8015357852426,
0.));
#11004=CARTESIAN_POINT('Ctrl Pts',(-11.5778153222435,-17.8015357852426,
21.));
#11005=CARTESIAN_POINT('Ctrl Pts',(-11.5333068279911,-17.7764940721306,
0.));
#11006=CARTESIAN_POINT('Ctrl Pts',(-11.5333068279911,-17.7764940721306,
21.));
#11007=CARTESIAN_POINT('Ctrl Pts',(-11.4889948016216,-17.7512577332768,
0.));
#11008=CARTESIAN_POINT('Ctrl Pts',(-11.4889948016216,-17.7512577332768,
21.));
#11009=CARTESIAN_POINT('Ctrl Pts',(-11.4448814046804,-17.725826190457,0.));
#11010=CARTESIAN_POINT('Ctrl Pts',(-11.4448814046804,-17.725826190457,21.));
#11011=CARTESIAN_POINT('Ctrl Pts',(-11.4009687970126,-17.700198872213,0.));
#11012=CARTESIAN_POINT('Ctrl Pts',(-11.4009687970126,-17.700198872213,21.));
#11013=CARTESIAN_POINT('Ctrl Pts',(-11.3572590796967,-17.674375235974,0.));
#11014=CARTESIAN_POINT('Ctrl Pts',(-11.3572590796967,-17.674375235974,21.));
#11015=CARTESIAN_POINT('Ctrl Pts',(-11.3137543310722,-17.6483547422688,
0.));
#11016=CARTESIAN_POINT('Ctrl Pts',(-11.3137543310722,-17.6483547422688,
21.));
#11017=CARTESIAN_POINT('Ctrl Pts',(-11.2704566868205,-17.6221368072528,
0.));
#11018=CARTESIAN_POINT('Ctrl Pts',(-11.2704566868205,-17.6221368072528,
21.));
#11019=CARTESIAN_POINT('Ctrl Pts',(-11.2273684103051,-17.5957207597803,
0.));
#11020=CARTESIAN_POINT('Ctrl Pts',(-11.2273684103051,-17.5957207597803,
21.));
#11021=CARTESIAN_POINT('Ctrl Pts',(-11.1844919535058,-17.5691058058227,
0.));
#11022=CARTESIAN_POINT('Ctrl Pts',(-11.1844919535058,-17.5691058058227,
21.));
#11023=CARTESIAN_POINT('Ctrl Pts',(-11.1418300507683,-17.5422909714139,
0.));
#11024=CARTESIAN_POINT('Ctrl Pts',(-11.1418300507683,-17.5422909714139,
21.));
#11025=CARTESIAN_POINT('Ctrl Pts',(-11.0993856581394,-17.5152751467292,
0.));
#11026=CARTESIAN_POINT('Ctrl Pts',(-11.0993856581394,-17.5152751467292,
21.));
#11027=CARTESIAN_POINT('Ctrl Pts',(-11.0571618040371,-17.4880571878157,
0.));
#11028=CARTESIAN_POINT('Ctrl Pts',(-11.0571618040371,-17.4880571878157,
21.));
#11029=CARTESIAN_POINT('Ctrl Pts',(-11.0151614525642,-17.460636011184,0.));
#11030=CARTESIAN_POINT('Ctrl Pts',(-11.0151614525642,-17.460636011184,21.));
#11031=CARTESIAN_POINT('Ctrl Pts',(-10.9733873885115,-17.4330106728622,
0.));
#11032=CARTESIAN_POINT('Ctrl Pts',(-10.9733873885115,-17.4330106728622,
21.));
#11033=CARTESIAN_POINT('Ctrl Pts',(-10.9318420203801,-17.4051805054129,
0.));
#11034=CARTESIAN_POINT('Ctrl Pts',(-10.9318420203801,-17.4051805054129,
21.));
#11035=CARTESIAN_POINT('Ctrl Pts',(-10.8905275295837,-17.377145012528,0.));
#11036=CARTESIAN_POINT('Ctrl Pts',(-10.8905275295837,-17.377145012528,21.));
#11037=CARTESIAN_POINT('Ctrl Pts',(-10.8494462423128,-17.3489036079991,
0.));
#11038=CARTESIAN_POINT('Ctrl Pts',(-10.8494462423128,-17.3489036079991,
21.));
#11039=CARTESIAN_POINT('Ctrl Pts',(-10.8086009632423,-17.3204553814537,
0.));
#11040=CARTESIAN_POINT('Ctrl Pts',(-10.8086009632423,-17.3204553814537,
21.));
#11041=CARTESIAN_POINT('Ctrl Pts',(-10.7679952591482,-17.2917988998581,
0.));
#11042=CARTESIAN_POINT('Ctrl Pts',(-10.7679952591482,-17.2917988998581,
21.));
#11043=CARTESIAN_POINT('Ctrl Pts',(-10.7276339231608,-17.2629318816279,
0.));
#11044=CARTESIAN_POINT('Ctrl Pts',(-10.7276339231608,-17.2629318816279,
21.));
#11045=CARTESIAN_POINT('Ctrl Pts',(-10.6875226650217,-17.2338514174708,
0.));
#11046=CARTESIAN_POINT('Ctrl Pts',(-10.6875226650217,-17.2338514174708,
21.));
#11047=CARTESIAN_POINT('Ctrl Pts',(-10.6476672831754,-17.2045545572011,
0.));
#11048=CARTESIAN_POINT('Ctrl Pts',(-10.6476672831754,-17.2045545572011,
21.));
#11049=CARTESIAN_POINT('Ctrl Pts',(-10.6080729180997,-17.1750388395657,
0.));
#11050=CARTESIAN_POINT('Ctrl Pts',(-10.6080729180997,-17.1750388395657,
21.));
#11051=CARTESIAN_POINT('Ctrl Pts',(-10.5687434234512,-17.1453027387554,
0.));
#11052=CARTESIAN_POINT('Ctrl Pts',(-10.5687434234512,-17.1453027387554,
21.));
#11053=CARTESIAN_POINT('Ctrl Pts',(-10.5296803023445,-17.1153464189932,
0.));
#11054=CARTESIAN_POINT('Ctrl Pts',(-10.5296803023445,-17.1153464189932,
21.));
#11055=CARTESIAN_POINT('Ctrl Pts',(-10.4908835057575,-17.0851711712016,
0.));
#11056=CARTESIAN_POINT('Ctrl Pts',(-10.4908835057575,-17.0851711712016,
21.));
#11057=CARTESIAN_POINT('Ctrl Pts',(-10.452353435089,-17.0547779975888,0.));
#11058=CARTESIAN_POINT('Ctrl Pts',(-10.452353435089,-17.0547779975888,21.));
#11059=CARTESIAN_POINT('Ctrl Pts',(-10.4140927470882,-17.0241663361802,
0.));
#11060=CARTESIAN_POINT('Ctrl Pts',(-10.4140927470882,-17.0241663361802,
21.));
#11061=CARTESIAN_POINT('Ctrl Pts',(-10.3761078860454,-16.9933329788855,
0.));
#11062=CARTESIAN_POINT('Ctrl Pts',(-10.3761078860454,-16.9933329788855,
21.));
#11063=CARTESIAN_POINT('Ctrl Pts',(-10.3384116178624,-16.9622702798438,
0.));
#11064=CARTESIAN_POINT('Ctrl Pts',(-10.3384116178624,-16.9622702798438,
21.));
#11065=CARTESIAN_POINT('Ctrl Pts',(-10.3010210756062,-16.9309675442425,
0.));
#11066=CARTESIAN_POINT('Ctrl Pts',(-10.3010210756062,-16.9309675442425,
21.));
#11067=CARTESIAN_POINT('Ctrl Pts',(-10.2639532144219,-16.8994142530447,
0.));
#11068=CARTESIAN_POINT('Ctrl Pts',(-10.2639532144219,-16.8994142530447,
21.));
#11069=CARTESIAN_POINT('Ctrl Pts',(-10.2272206796636,-16.8676029947679,
0.));
#11070=CARTESIAN_POINT('Ctrl Pts',(-10.2272206796636,-16.8676029947679,
21.));
#11071=CARTESIAN_POINT('Ctrl Pts',(-10.1908283166713,-16.8355319435838,
0.));
#11072=CARTESIAN_POINT('Ctrl Pts',(-10.1908283166713,-16.8355319435838,
21.));
#11073=CARTESIAN_POINT('Ctrl Pts',(-10.1547673397274,-16.8032089941901,
0.));
#11074=CARTESIAN_POINT('Ctrl Pts',(-10.1547673397274,-16.8032089941901,
21.));
#11075=CARTESIAN_POINT('Ctrl Pts',(-10.1190207721353,-16.7706479198888,
0.));
#11076=CARTESIAN_POINT('Ctrl Pts',(-10.1190207721353,-16.7706479198888,
21.));
#11077=CARTESIAN_POINT('Ctrl Pts',(-10.0835742491038,-16.7378607357337,
0.));
#11078=CARTESIAN_POINT('Ctrl Pts',(-10.0835742491038,-16.7378607357337,
21.));
#11079=CARTESIAN_POINT('Ctrl Pts',(-10.0484259314257,-16.7048506904207,
0.));
#11080=CARTESIAN_POINT('Ctrl Pts',(-10.0484259314257,-16.7048506904207,
21.));
#11081=CARTESIAN_POINT('Ctrl Pts',(-10.0135950379525,-16.6716062376277,
0.));
#11082=CARTESIAN_POINT('Ctrl Pts',(-10.0135950379525,-16.6716062376277,
21.));
#11083=CARTESIAN_POINT('Ctrl Pts',(-9.97913546489641,-16.6380914029057,
0.));
#11084=CARTESIAN_POINT('Ctrl Pts',(-9.97913546489641,-16.6380914029057,
21.));
#11085=CARTESIAN_POINT('Ctrl Pts',(-9.9451214271291,-16.6042559779574,0.));
#11086=CARTESIAN_POINT('Ctrl Pts',(-9.9451214271291,-16.6042559779574,21.));
#11087=CARTESIAN_POINT('Ctrl Pts',(-9.91162317616649,-16.5700527532381,
0.));
#11088=CARTESIAN_POINT('Ctrl Pts',(-9.91162317616649,-16.5700527532381,
21.));
#11089=CARTESIAN_POINT('Ctrl Pts',(-9.8786843754698,-16.5354535643506,0.));
#11090=CARTESIAN_POINT('Ctrl Pts',(-9.8786843754698,-16.5354535643506,21.));
#11091=CARTESIAN_POINT('Ctrl Pts',(-9.84630229363522,-16.5004633692332,
0.));
#11092=CARTESIAN_POINT('Ctrl Pts',(-9.84630229363522,-16.5004633692332,
21.));
#11093=CARTESIAN_POINT('Ctrl Pts',(-9.81439757053279,-16.4651416449558,
0.));
#11094=CARTESIAN_POINT('Ctrl Pts',(-9.81439757053279,-16.4651416449558,
21.));
#11095=CARTESIAN_POINT('Ctrl Pts',(-9.78285689698057,-16.4295725710378,
0.));
#11096=CARTESIAN_POINT('Ctrl Pts',(-9.78285689698057,-16.4295725710378,
21.));
#11097=CARTESIAN_POINT('Ctrl Pts',(-9.75159288382685,-16.3938231282759,
0.));
#11098=CARTESIAN_POINT('Ctrl Pts',(-9.75159288382685,-16.3938231282759,
21.));
#11099=CARTESIAN_POINT('Ctrl Pts',(-9.72060002001012,-16.3579039682519,
0.));
#11100=CARTESIAN_POINT('Ctrl Pts',(-9.72060002001012,-16.3579039682519,
21.));
#11101=CARTESIAN_POINT('Ctrl Pts',(-9.69000797146315,-16.3217321000366,
0.));
#11102=CARTESIAN_POINT('Ctrl Pts',(-9.69000797146315,-16.3217321000366,
21.));
#11103=CARTESIAN_POINT('Ctrl Pts',(-9.66014786078746,-16.2850845948324,
0.));
#11104=CARTESIAN_POINT('Ctrl Pts',(-9.66014786078746,-16.2850845948324,
21.));
#11105=CARTESIAN_POINT('Ctrl Pts',(-9.63146315443273,-16.2476599387841,
0.));
#11106=CARTESIAN_POINT('Ctrl Pts',(-9.63146315443273,-16.2476599387841,
21.));
#11107=CARTESIAN_POINT('Ctrl Pts',(-9.60981421781524,-16.2168537871666,
0.));
#11108=CARTESIAN_POINT('Ctrl Pts',(-9.60981421781524,-16.2168537871666,
21.));
#11109=CARTESIAN_POINT('Ctrl Pts',(-9.59446643316597,-16.1931534965272,
0.));
#11110=CARTESIAN_POINT('Ctrl Pts',(-9.59446643316597,-16.1931534965272,
21.));
#11111=CARTESIAN_POINT('Ctrl Pts',(-9.58464985151483,-16.1770747160769,
0.));
#11112=CARTESIAN_POINT('Ctrl Pts',(-9.58464985151483,-16.1770747160769,
21.));
#11113=CARTESIAN_POINT('Ctrl Pts',(-9.57984538049455,-16.1689656784104,
0.));
#11114=CARTESIAN_POINT('Ctrl Pts',(-9.57984538049455,-16.1689656784104,
21.));
#11115=CARTESIAN_POINT('',(-12.3627494547114,-18.1978687191669,0.));
#11116=CARTESIAN_POINT('Ctrl Pts',(-9.57984538049455,-16.1689656784104,
0.));
#11117=CARTESIAN_POINT('Ctrl Pts',(-9.58464985151483,-16.1770747160769,
0.));
#11118=CARTESIAN_POINT('Ctrl Pts',(-9.59446643316597,-16.1931534965272,
0.));
#11119=CARTESIAN_POINT('Ctrl Pts',(-9.60981421781524,-16.2168537871666,
0.));
#11120=CARTESIAN_POINT('Ctrl Pts',(-9.63146315443273,-16.2476599387841,
0.));
#11121=CARTESIAN_POINT('Ctrl Pts',(-9.66014786078746,-16.2850845948324,
0.));
#11122=CARTESIAN_POINT('Ctrl Pts',(-9.69000797146315,-16.3217321000366,
0.));
#11123=CARTESIAN_POINT('Ctrl Pts',(-9.72060002001012,-16.3579039682519,
0.));
#11124=CARTESIAN_POINT('Ctrl Pts',(-9.75159288382685,-16.3938231282759,
0.));
#11125=CARTESIAN_POINT('Ctrl Pts',(-9.78285689698057,-16.4295725710378,
0.));
#11126=CARTESIAN_POINT('Ctrl Pts',(-9.81439757053279,-16.4651416449558,
0.));
#11127=CARTESIAN_POINT('Ctrl Pts',(-9.84630229363522,-16.5004633692332,
0.));
#11128=CARTESIAN_POINT('Ctrl Pts',(-9.8786843754698,-16.5354535643506,0.));
#11129=CARTESIAN_POINT('Ctrl Pts',(-9.91162317616649,-16.5700527532381,
0.));
#11130=CARTESIAN_POINT('Ctrl Pts',(-9.9451214271291,-16.6042559779574,0.));
#11131=CARTESIAN_POINT('Ctrl Pts',(-9.97913546489641,-16.6380914029057,
0.));
#11132=CARTESIAN_POINT('Ctrl Pts',(-10.0135950379525,-16.6716062376277,
0.));
#11133=CARTESIAN_POINT('Ctrl Pts',(-10.0484259314257,-16.7048506904207,
0.));
#11134=CARTESIAN_POINT('Ctrl Pts',(-10.0835742491038,-16.7378607357337,
0.));
#11135=CARTESIAN_POINT('Ctrl Pts',(-10.1190207721353,-16.7706479198888,
0.));
#11136=CARTESIAN_POINT('Ctrl Pts',(-10.1547673397274,-16.8032089941901,
0.));
#11137=CARTESIAN_POINT('Ctrl Pts',(-10.1908283166713,-16.8355319435838,
0.));
#11138=CARTESIAN_POINT('Ctrl Pts',(-10.2272206796636,-16.8676029947679,
0.));
#11139=CARTESIAN_POINT('Ctrl Pts',(-10.2639532144219,-16.8994142530447,
0.));
#11140=CARTESIAN_POINT('Ctrl Pts',(-10.3010210756062,-16.9309675442425,
0.));
#11141=CARTESIAN_POINT('Ctrl Pts',(-10.3384116178624,-16.9622702798438,
0.));
#11142=CARTESIAN_POINT('Ctrl Pts',(-10.3761078860454,-16.9933329788855,
0.));
#11143=CARTESIAN_POINT('Ctrl Pts',(-10.4140927470882,-17.0241663361802,
0.));
#11144=CARTESIAN_POINT('Ctrl Pts',(-10.452353435089,-17.0547779975888,0.));
#11145=CARTESIAN_POINT('Ctrl Pts',(-10.4908835057575,-17.0851711712016,
0.));
#11146=CARTESIAN_POINT('Ctrl Pts',(-10.5296803023445,-17.1153464189932,
0.));
#11147=CARTESIAN_POINT('Ctrl Pts',(-10.5687434234512,-17.1453027387554,
0.));
#11148=CARTESIAN_POINT('Ctrl Pts',(-10.6080729180997,-17.1750388395657,
0.));
#11149=CARTESIAN_POINT('Ctrl Pts',(-10.6476672831754,-17.2045545572011,
0.));
#11150=CARTESIAN_POINT('Ctrl Pts',(-10.6875226650217,-17.2338514174708,
0.));
#11151=CARTESIAN_POINT('Ctrl Pts',(-10.7276339231608,-17.2629318816279,
0.));
#11152=CARTESIAN_POINT('Ctrl Pts',(-10.7679952591482,-17.2917988998581,
0.));
#11153=CARTESIAN_POINT('Ctrl Pts',(-10.8086009632423,-17.3204553814537,
0.));
#11154=CARTESIAN_POINT('Ctrl Pts',(-10.8494462423128,-17.3489036079991,
0.));
#11155=CARTESIAN_POINT('Ctrl Pts',(-10.8905275295837,-17.377145012528,0.));
#11156=CARTESIAN_POINT('Ctrl Pts',(-10.9318420203801,-17.4051805054129,
0.));
#11157=CARTESIAN_POINT('Ctrl Pts',(-10.9733873885115,-17.4330106728622,
0.));
#11158=CARTESIAN_POINT('Ctrl Pts',(-11.0151614525642,-17.460636011184,0.));
#11159=CARTESIAN_POINT('Ctrl Pts',(-11.0571618040371,-17.4880571878157,
0.));
#11160=CARTESIAN_POINT('Ctrl Pts',(-11.0993856581394,-17.5152751467292,
0.));
#11161=CARTESIAN_POINT('Ctrl Pts',(-11.1418300507683,-17.5422909714139,
0.));
#11162=CARTESIAN_POINT('Ctrl Pts',(-11.1844919535058,-17.5691058058227,
0.));
#11163=CARTESIAN_POINT('Ctrl Pts',(-11.2273684103051,-17.5957207597803,
0.));
#11164=CARTESIAN_POINT('Ctrl Pts',(-11.2704566868205,-17.6221368072528,
0.));
#11165=CARTESIAN_POINT('Ctrl Pts',(-11.3137543310722,-17.6483547422688,
0.));
#11166=CARTESIAN_POINT('Ctrl Pts',(-11.3572590796967,-17.674375235974,0.));
#11167=CARTESIAN_POINT('Ctrl Pts',(-11.4009687970126,-17.700198872213,0.));
#11168=CARTESIAN_POINT('Ctrl Pts',(-11.4448814046804,-17.725826190457,0.));
#11169=CARTESIAN_POINT('Ctrl Pts',(-11.4889948016216,-17.7512577332768,
0.));
#11170=CARTESIAN_POINT('Ctrl Pts',(-11.5333068279911,-17.7764940721306,
0.));
#11171=CARTESIAN_POINT('Ctrl Pts',(-11.5778153222435,-17.8015357852426,
0.));
#11172=CARTESIAN_POINT('Ctrl Pts',(-11.6225181583564,-17.8263834470057,
0.));
#11173=CARTESIAN_POINT('Ctrl Pts',(-11.6674132861792,-17.8510376144926,
0.));
#11174=CARTESIAN_POINT('Ctrl Pts',(-11.7124987772363,-17.8754988158862,
0.));
#11175=CARTESIAN_POINT('Ctrl Pts',(-11.7577728408871,-17.8997675418752,
0.));
#11176=CARTESIAN_POINT('Ctrl Pts',(-11.8032337607271,-17.9238442458356,
0.));
#11177=CARTESIAN_POINT('Ctrl Pts',(-11.8488798430201,-17.9477293432951,
0.));
#11178=CARTESIAN_POINT('Ctrl Pts',(-11.8947093631895,-17.9714232133203,
0.));
#11179=CARTESIAN_POINT('Ctrl Pts',(-11.9407205019619,-17.9949261997754,
0.));
#11180=CARTESIAN_POINT('Ctrl Pts',(-11.986911314246,-18.0182386160553,0.));
#11181=CARTESIAN_POINT('Ctrl Pts',(-12.0332798395991,-18.0413607600052,
0.));
#11182=CARTESIAN_POINT('Ctrl Pts',(-12.0798241915081,-18.0642929289333,
0.));
#11183=CARTESIAN_POINT('Ctrl Pts',(-12.1265426519718,-18.0870354350128,
0.));
#11184=CARTESIAN_POINT('Ctrl Pts',(-12.1734337668195,-18.109588624154,0.));
#11185=CARTESIAN_POINT('Ctrl Pts',(-12.2299089600472,-18.1364257412858,
0.));
#11186=CARTESIAN_POINT('Ctrl Pts',(-12.2771850498068,-18.1585543320743,
0.));
#11187=CARTESIAN_POINT('Ctrl Pts',(-12.3151419520839,-18.1761067306718,
0.));
#11188=CARTESIAN_POINT('Ctrl Pts',(-12.3436860694314,-18.1891864723772,
0.));
#11189=CARTESIAN_POINT('Ctrl Pts',(-12.3627494547115,-18.1978687191668,
0.));
#11190=CARTESIAN_POINT('',(-12.3627494547114,-18.1978687191669,13.));
#11191=CARTESIAN_POINT('Ctrl Pts',(-12.3627494547115,-18.1978687191668,
13.));
#11192=CARTESIAN_POINT('Ctrl Pts',(-12.2689088964153,-18.1551298837072,
13.));
#11193=CARTESIAN_POINT('Ctrl Pts',(-12.1760519707549,-18.111299637656,13.));
#11194=CARTESIAN_POINT('Ctrl Pts',(-12.0842021157222,-18.0663670681848,
13.));
#11195=CARTESIAN_POINT('Ctrl Pts',(-11.9320029094011,-17.9919118454842,
13.));
#11196=CARTESIAN_POINT('Ctrl Pts',(-11.7825824042094,-17.9144310022929,
13.));
#11197=CARTESIAN_POINT('Ctrl Pts',(-11.6362239728201,-17.8338669529311,
13.));
#11198=CARTESIAN_POINT('Ctrl Pts',(-11.523724298462,-17.7719406994714,13.));
#11199=CARTESIAN_POINT('Ctrl Pts',(-11.4130324604454,-17.708190453754,13.));
#11200=CARTESIAN_POINT('Ctrl Pts',(-11.3042990938976,-17.6425762029941,
13.));
#11201=CARTESIAN_POINT('Ctrl Pts',(-11.1872502400868,-17.571944040219,13.));
#11202=CARTESIAN_POINT('Ctrl Pts',(-11.0724652191949,-17.499154807149,13.));
#11203=CARTESIAN_POINT('Ctrl Pts',(-10.9601920980076,-17.4241207695605,
13.));
#11204=CARTESIAN_POINT('Ctrl Pts',(-10.8980346540897,-17.3825798919753,
13.));
#11205=CARTESIAN_POINT('Ctrl Pts',(-10.8366430107889,-17.3403540655037,
13.));
#11206=CARTESIAN_POINT('Ctrl Pts',(-10.7760628634082,-17.2974271318847,
13.));
#11207=CARTESIAN_POINT('Ctrl Pts',(-10.71768544558,-17.2560610466519,13.));
#11208=CARTESIAN_POINT('Ctrl Pts',(-10.6600671046061,-17.2140399833079,
13.));
#11209=CARTESIAN_POINT('Ctrl Pts',(-10.6032772242041,-17.1713305004863,
13.));
#11210=CARTESIAN_POINT('Ctrl Pts',(-10.5541933587631,-17.1344164148599,
13.));
#11211=CARTESIAN_POINT('Ctrl Pts',(-10.5057257098335,-17.096989955235,13.));
#11212=CARTESIAN_POINT('Ctrl Pts',(-10.4578814177545,-17.0590571075016,
13.));
#11213=CARTESIAN_POINT('Ctrl Pts',(-10.423545733757,-17.0318344187272,13.));
#11214=CARTESIAN_POINT('Ctrl Pts',(-10.3895287972434,-17.004352569251,13.));
#11215=CARTESIAN_POINT('Ctrl Pts',(-10.3558648787318,-16.9765917293735,
13.));
#11216=CARTESIAN_POINT('Ctrl Pts',(-10.3227491363857,-16.9492829411712,
13.));
#11217=CARTESIAN_POINT('Ctrl Pts',(-10.2899802165512,-16.9217004795811,
13.));
#11218=CARTESIAN_POINT('Ctrl Pts',(-10.257603002843,-16.8938171684013,13.));
#11219=CARTESIAN_POINT('Ctrl Pts',(-10.2295300560935,-16.8696406992028,
13.));
#11220=CARTESIAN_POINT('Ctrl Pts',(-10.2017536135352,-16.8452366235594,
13.));
#11221=CARTESIAN_POINT('Ctrl Pts',(-10.1742626909659,-16.8206160301345,
13.));
#11222=CARTESIAN_POINT('Ctrl Pts',(-10.1493622215735,-16.7983154204895,
13.));
#11223=CARTESIAN_POINT('Ctrl Pts',(-10.1246914564006,-16.7758403904972,
13.));
#11224=CARTESIAN_POINT('Ctrl Pts',(-10.1002324979069,-16.7532063442149,
13.));
#11225=CARTESIAN_POINT('Ctrl Pts',(-10.079629563683,-16.7341406196096,13.));
#11226=CARTESIAN_POINT('Ctrl Pts',(-10.0591755003946,-16.7149630708293,
13.));
#11227=CARTESIAN_POINT('Ctrl Pts',(-10.0388873687047,-16.6956634327229,
13.));
#11228=CARTESIAN_POINT('Ctrl Pts',(-10.0095282357399,-16.6677347574757,
13.));
#11229=CARTESIAN_POINT('Ctrl Pts',(-9.98051721208624,-16.6395499070626,
13.));
#11230=CARTESIAN_POINT('Ctrl Pts',(-9.95203577377263,-16.6109867038064,
13.));
#11231=CARTESIAN_POINT('Ctrl Pts',(-9.9348261830604,-16.5937277075416,13.));
#11232=CARTESIAN_POINT('Ctrl Pts',(-9.91781279953151,-16.5763285722608,
13.));
#11233=CARTESIAN_POINT('Ctrl Pts',(-9.90101792991858,-16.5587751451304,
13.));
#11234=CARTESIAN_POINT('Ctrl Pts',(-9.88552833553625,-16.5425859473257,
13.));
#11235=CARTESIAN_POINT('Ctrl Pts',(-9.87022569084434,-16.5262647433908,
13.));
#11236=CARTESIAN_POINT('Ctrl Pts',(-9.85509024411449,-16.5098269904329,
13.));
#11237=CARTESIAN_POINT('Ctrl Pts',(-9.83426990258338,-16.4872151946467,
13.));
#11238=CARTESIAN_POINT('Ctrl Pts',(-9.81375991310154,-16.4643869859202,
13.));
#11239=CARTESIAN_POINT('Ctrl Pts',(-9.7934396802235,-16.4414328801903,13.));
#11240=CARTESIAN_POINT('Ctrl Pts',(-9.7805481624305,-16.4268703865311,13.));
#11241=CARTESIAN_POINT('Ctrl Pts',(-9.76773166757831,-16.4122582103724,
13.));
#11242=CARTESIAN_POINT('Ctrl Pts',(-9.75498419478216,-16.3976025796313,
13.));
#11243=CARTESIAN_POINT('Ctrl Pts',(-9.74354393127652,-16.3844498331849,
13.));
#11244=CARTESIAN_POINT('Ctrl Pts',(-9.73215866496981,-16.3712625079592,
13.));
#11245=CARTESIAN_POINT('Ctrl Pts',(-9.72085751043954,-16.3580219469452,
13.));
#11246=CARTESIAN_POINT('Ctrl Pts',(-9.70897774622862,-16.3441034802572,
13.));
#11247=CARTESIAN_POINT('Ctrl Pts',(-9.69719080116679,-16.330126283354,13.));
#11248=CARTESIAN_POINT('Ctrl Pts',(-9.68558166507924,-16.3160331239166,
13.));
#11249=CARTESIAN_POINT('Ctrl Pts',(-9.66629891585391,-16.292624417431,13.));
#11250=CARTESIAN_POINT('Ctrl Pts',(-9.64751373148189,-16.268891093964,13.));
#11251=CARTESIAN_POINT('Ctrl Pts',(-9.62974342615828,-16.2444806681934,
13.));
#11252=CARTESIAN_POINT('Ctrl Pts',(-9.61994424733045,-16.231019890619,13.));
#11253=CARTESIAN_POINT('Ctrl Pts',(-9.61045478083913,-16.2173524098339,
13.));
#11254=CARTESIAN_POINT('Ctrl Pts',(-9.60133856554245,-16.2034347659916,
13.));
#11255=CARTESIAN_POINT('Ctrl Pts',(-9.59392299464928,-16.1921134806533,
13.));
#11256=CARTESIAN_POINT('Ctrl Pts',(-9.58675434324541,-16.1806266997688,
13.));
#11257=CARTESIAN_POINT('Ctrl Pts',(-9.57984538049455,-16.1689656784104,
13.));
#11258=CARTESIAN_POINT('',(-12.3627494547114,-18.1978687191669,0.));
#11259=CARTESIAN_POINT('Origin',(-3.33073116609659E-12,-4.58435815896522E-12,
0.));
#11260=CARTESIAN_POINT('',(-13.4869019493419,-17.3811241238545,0.));
#11261=CARTESIAN_POINT('Origin',(-3.33073116609659E-12,-4.58435815896522E-12,
0.));
#11262=CARTESIAN_POINT('',(-13.4869019493419,-17.3811241238545,13.));
#11263=CARTESIAN_POINT('Origin',(-3.33073116609659E-12,-4.58435815896522E-12,
13.));
#11264=CARTESIAN_POINT('',(-13.4869019493419,-17.3811241238545,0.));
#11265=CARTESIAN_POINT('Ctrl Pts',(-12.4172651441477,-14.1074595503134,
0.));
#11266=CARTESIAN_POINT('Ctrl Pts',(-12.4172651441477,-14.1074595503134,
21.));
#11267=CARTESIAN_POINT('Ctrl Pts',(-12.4234926340671,-14.1145347042316,
0.));
#11268=CARTESIAN_POINT('Ctrl Pts',(-12.4234926340671,-14.1145347042316,
21.));
#11269=CARTESIAN_POINT('Ctrl Pts',(-12.4357509724316,-14.1288394445866,
0.));
#11270=CARTESIAN_POINT('Ctrl Pts',(-12.4357509724316,-14.1288394445866,
21.));
#11271=CARTESIAN_POINT('Ctrl Pts',(-12.4535485619996,-14.1507598477672,
0.));
#11272=CARTESIAN_POINT('Ctrl Pts',(-12.4535485619996,-14.1507598477672,
21.));
#11273=CARTESIAN_POINT('Ctrl Pts',(-12.4761570639125,-14.1808688343892,
0.));
#11274=CARTESIAN_POINT('Ctrl Pts',(-12.4761570639125,-14.1808688343892,
21.));
#11275=CARTESIAN_POINT('Ctrl Pts',(-12.5028859651751,-14.2197144660135,
0.));
#11276=CARTESIAN_POINT('Ctrl Pts',(-12.5028859651751,-14.2197144660135,
21.));
#11277=CARTESIAN_POINT('Ctrl Pts',(-12.5285125321527,-14.2594378207584,
0.));
#11278=CARTESIAN_POINT('Ctrl Pts',(-12.5285125321527,-14.2594378207584,
21.));
#11279=CARTESIAN_POINT('Ctrl Pts',(-12.5534605602317,-14.2997103098726,
0.));
#11280=CARTESIAN_POINT('Ctrl Pts',(-12.5534605602317,-14.2997103098726,
21.));
#11281=CARTESIAN_POINT('Ctrl Pts',(-12.5780443898087,-14.3402859058353,
0.));
#11282=CARTESIAN_POINT('Ctrl Pts',(-12.5780443898087,-14.3402859058353,
21.));
#11283=CARTESIAN_POINT('Ctrl Pts',(-12.6023830189244,-14.3810669346235,
0.));
#11284=CARTESIAN_POINT('Ctrl Pts',(-12.6023830189244,-14.3810669346235,
21.));
#11285=CARTESIAN_POINT('Ctrl Pts',(-12.626464614311,-14.4220553460485,0.));
#11286=CARTESIAN_POINT('Ctrl Pts',(-12.626464614311,-14.4220553460485,21.));
#11287=CARTESIAN_POINT('Ctrl Pts',(-12.6501984687124,-14.463313553928,0.));
#11288=CARTESIAN_POINT('Ctrl Pts',(-12.6501984687124,-14.463313553928,21.));
#11289=CARTESIAN_POINT('Ctrl Pts',(-12.6734695081852,-14.5049233087958,
0.));
#11290=CARTESIAN_POINT('Ctrl Pts',(-12.6734695081852,-14.5049233087958,
21.));
#11291=CARTESIAN_POINT('Ctrl Pts',(-12.6961966430455,-14.5469417071951,
0.));
#11292=CARTESIAN_POINT('Ctrl Pts',(-12.6961966430455,-14.5469417071951,
21.));
#11293=CARTESIAN_POINT('Ctrl Pts',(-12.7183743139638,-14.5893698147583,
0.));
#11294=CARTESIAN_POINT('Ctrl Pts',(-12.7183743139638,-14.5893698147583,
21.));
#11295=CARTESIAN_POINT('Ctrl Pts',(-12.7400427996251,-14.6321748083434,
0.));
#11296=CARTESIAN_POINT('Ctrl Pts',(-12.7400427996251,-14.6321748083434,
21.));
#11297=CARTESIAN_POINT('Ctrl Pts',(-12.7612687078867,-14.6753044633399,
0.));
#11298=CARTESIAN_POINT('Ctrl Pts',(-12.7612687078867,-14.6753044633399,
21.));
#11299=CARTESIAN_POINT('Ctrl Pts',(-12.7821227233337,-14.7187037124277,
0.));
#11300=CARTESIAN_POINT('Ctrl Pts',(-12.7821227233337,-14.7187037124277,
21.));
#11301=CARTESIAN_POINT('Ctrl Pts',(-12.8026557145457,-14.7623324139791,
0.));
#11302=CARTESIAN_POINT('Ctrl Pts',(-12.8026557145457,-14.7623324139791,
21.));
#11303=CARTESIAN_POINT('Ctrl Pts',(-12.8228846016791,-14.8061758577898,
0.));
#11304=CARTESIAN_POINT('Ctrl Pts',(-12.8228846016791,-14.8061758577898,
21.));
#11305=CARTESIAN_POINT('Ctrl Pts',(-12.8428057266944,-14.8502347891476,
0.));
#11306=CARTESIAN_POINT('Ctrl Pts',(-12.8428057266944,-14.8502347891476,
21.));
#11307=CARTESIAN_POINT('Ctrl Pts',(-12.8624032236317,-14.8945191569251,
0.));
#11308=CARTESIAN_POINT('Ctrl Pts',(-12.8624032236317,-14.8945191569251,
21.));
#11309=CARTESIAN_POINT('Ctrl Pts',(-12.8816587472147,-14.9390408507356,
0.));
#11310=CARTESIAN_POINT('Ctrl Pts',(-12.8816587472147,-14.9390408507356,
21.));
#11311=CARTESIAN_POINT('Ctrl Pts',(-12.9005620742036,-14.9838057866976,
0.));
#11312=CARTESIAN_POINT('Ctrl Pts',(-12.9005620742036,-14.9838057866976,
21.));
#11313=CARTESIAN_POINT('Ctrl Pts',(-12.9191164383568,-15.0288099208306,
0.));
#11314=CARTESIAN_POINT('Ctrl Pts',(-12.9191164383568,-15.0288099208306,
21.));
#11315=CARTESIAN_POINT('Ctrl Pts',(-12.9373327960422,-15.0740435169624,
0.));
#11316=CARTESIAN_POINT('Ctrl Pts',(-12.9373327960422,-15.0740435169624,
21.));
#11317=CARTESIAN_POINT('Ctrl Pts',(-12.9552263908864,-15.1194937003528,
0.));
#11318=CARTESIAN_POINT('Ctrl Pts',(-12.9552263908864,-15.1194937003528,
21.));
#11319=CARTESIAN_POINT('Ctrl Pts',(-12.9728126886697,-15.1651474813659,
0.));
#11320=CARTESIAN_POINT('Ctrl Pts',(-12.9728126886697,-15.1651474813659,
21.));
#11321=CARTESIAN_POINT('Ctrl Pts',(-12.9901029059182,-15.2109950816083,
0.));
#11322=CARTESIAN_POINT('Ctrl Pts',(-12.9901029059182,-15.2109950816083,
21.));
#11323=CARTESIAN_POINT('Ctrl Pts',(-13.0071020851025,-15.2570313635503,
0.));
#11324=CARTESIAN_POINT('Ctrl Pts',(-13.0071020851025,-15.2570313635503,
21.));
#11325=CARTESIAN_POINT('Ctrl Pts',(-13.0238115816728,-15.3032539741328,
0.));
#11326=CARTESIAN_POINT('Ctrl Pts',(-13.0238115816728,-15.3032539741328,
21.));
#11327=CARTESIAN_POINT('Ctrl Pts',(-13.0402305665115,-15.3496622219036,
0.));
#11328=CARTESIAN_POINT('Ctrl Pts',(-13.0402305665115,-15.3496622219036,
21.));
#11329=CARTESIAN_POINT('Ctrl Pts',(-13.0563577967298,-15.3962557545684,
0.));
#11330=CARTESIAN_POINT('Ctrl Pts',(-13.0563577967298,-15.3962557545684,
21.));
#11331=CARTESIAN_POINT('Ctrl Pts',(-13.0721935806302,-15.4430330918328,
0.));
#11332=CARTESIAN_POINT('Ctrl Pts',(-13.0721935806302,-15.4430330918328,
21.));
#11333=CARTESIAN_POINT('Ctrl Pts',(-13.087740560189,-15.4899910401523,0.));
#11334=CARTESIAN_POINT('Ctrl Pts',(-13.087740560189,-15.4899910401523,21.));
#11335=CARTESIAN_POINT('Ctrl Pts',(-13.1030026646917,-15.5371254712111,
0.));
#11336=CARTESIAN_POINT('Ctrl Pts',(-13.1030026646917,-15.5371254712111,
21.));
#11337=CARTESIAN_POINT('Ctrl Pts',(-13.1179844917497,-15.5844317820184,
0.));
#11338=CARTESIAN_POINT('Ctrl Pts',(-13.1179844917497,-15.5844317820184,
21.));
#11339=CARTESIAN_POINT('Ctrl Pts',(-13.1326905726717,-15.6319054413079,
0.));
#11340=CARTESIAN_POINT('Ctrl Pts',(-13.1326905726717,-15.6319054413079,
21.));
#11341=CARTESIAN_POINT('Ctrl Pts',(-13.147124558532,-15.6795425955901,0.));
#11342=CARTESIAN_POINT('Ctrl Pts',(-13.147124558532,-15.6795425955901,21.));
#11343=CARTESIAN_POINT('Ctrl Pts',(-13.161288914421,-15.7273402954914,0.));
#11344=CARTESIAN_POINT('Ctrl Pts',(-13.161288914421,-15.7273402954914,21.));
#11345=CARTESIAN_POINT('Ctrl Pts',(-13.1751853728467,-15.7752961549278,
0.));
#11346=CARTESIAN_POINT('Ctrl Pts',(-13.1751853728467,-15.7752961549278,
21.));
#11347=CARTESIAN_POINT('Ctrl Pts',(-13.1888152101588,-15.8234081427091,
0.));
#11348=CARTESIAN_POINT('Ctrl Pts',(-13.1888152101588,-15.8234081427091,
21.));
#11349=CARTESIAN_POINT('Ctrl Pts',(-13.2021795724682,-15.8716743375555,
0.));
#11350=CARTESIAN_POINT('Ctrl Pts',(-13.2021795724682,-15.8716743375555,
21.));
#11351=CARTESIAN_POINT('Ctrl Pts',(-13.2152798388134,-15.9200926550954,
0.));
#11352=CARTESIAN_POINT('Ctrl Pts',(-13.2152798388134,-15.9200926550954,
21.));
#11353=CARTESIAN_POINT('Ctrl Pts',(-13.2281177675127,-15.9686607385389,
0.));
#11354=CARTESIAN_POINT('Ctrl Pts',(-13.2281177675127,-15.9686607385389,
21.));
#11355=CARTESIAN_POINT('Ctrl Pts',(-13.240695304984,-16.0173761036734,0.));
#11356=CARTESIAN_POINT('Ctrl Pts',(-13.240695304984,-16.0173761036734,21.));
#11357=CARTESIAN_POINT('Ctrl Pts',(-13.2530144750236,-16.0662362238032,
0.));
#11358=CARTESIAN_POINT('Ctrl Pts',(-13.2530144750236,-16.0662362238032,
21.));
#11359=CARTESIAN_POINT('Ctrl Pts',(-13.2650772466062,-16.1152386305152,
0.));
#11360=CARTESIAN_POINT('Ctrl Pts',(-13.2650772466062,-16.1152386305152,
21.));
#11361=CARTESIAN_POINT('Ctrl Pts',(-13.2768853909882,-16.1643810242643,
0.));
#11362=CARTESIAN_POINT('Ctrl Pts',(-13.2768853909882,-16.1643810242643,
21.));
#11363=CARTESIAN_POINT('Ctrl Pts',(-13.2884404210388,-16.2136613184475,
0.));
#11364=CARTESIAN_POINT('Ctrl Pts',(-13.2884404210388,-16.2136613184475,
21.));
#11365=CARTESIAN_POINT('Ctrl Pts',(-13.2997436744733,-16.2630775678735,
0.));
#11366=CARTESIAN_POINT('Ctrl Pts',(-13.2997436744733,-16.2630775678735,
21.));
#11367=CARTESIAN_POINT('Ctrl Pts',(-13.3107963665229,-16.3126279218067,
0.));
#11368=CARTESIAN_POINT('Ctrl Pts',(-13.3107963665229,-16.3126279218067,
21.));
#11369=CARTESIAN_POINT('Ctrl Pts',(-13.3215996524974,-16.3623105703343,
0.));
#11370=CARTESIAN_POINT('Ctrl Pts',(-13.3215996524974,-16.3623105703343,
21.));
#11371=CARTESIAN_POINT('Ctrl Pts',(-13.3321546976812,-16.4121236828756,
0.));
#11372=CARTESIAN_POINT('Ctrl Pts',(-13.3321546976812,-16.4121236828756,
21.));
#11373=CARTESIAN_POINT('Ctrl Pts',(-13.3424627129921,-16.4620653818862,
0.));
#11374=CARTESIAN_POINT('Ctrl Pts',(-13.3424627129921,-16.4620653818862,
21.));
#11375=CARTESIAN_POINT('Ctrl Pts',(-13.3525249163084,-16.5121337902953,
0.));
#11376=CARTESIAN_POINT('Ctrl Pts',(-13.3525249163084,-16.5121337902953,
21.));
#11377=CARTESIAN_POINT('Ctrl Pts',(-13.3623425108873,-16.5623270636327,
0.));
#11378=CARTESIAN_POINT('Ctrl Pts',(-13.3623425108873,-16.5623270636327,
21.));
#11379=CARTESIAN_POINT('Ctrl Pts',(-13.3719166600676,-16.612643424234,0.));
#11380=CARTESIAN_POINT('Ctrl Pts',(-13.3719166600676,-16.612643424234,21.));
#11381=CARTESIAN_POINT('Ctrl Pts',(-13.381248462113,-16.6630812012276,0.));
#11382=CARTESIAN_POINT('Ctrl Pts',(-13.381248462113,-16.6630812012276,21.));
#11383=CARTESIAN_POINT('Ctrl Pts',(-13.3903389370346,-16.7136388432444,
0.));
#11384=CARTESIAN_POINT('Ctrl Pts',(-13.3903389370346,-16.7136388432444,
21.));
#11385=CARTESIAN_POINT('Ctrl Pts',(-13.3991890464165,-16.7643148579872,
0.));
#11386=CARTESIAN_POINT('Ctrl Pts',(-13.3991890464165,-16.7643148579872,
21.));
#11387=CARTESIAN_POINT('Ctrl Pts',(-13.4077997088426,-16.8151077630226,
0.));
#11388=CARTESIAN_POINT('Ctrl Pts',(-13.4077997088426,-16.8151077630226,
21.));
#11389=CARTESIAN_POINT('Ctrl Pts',(-13.4161718177499,-16.8660160353187,
0.));
#11390=CARTESIAN_POINT('Ctrl Pts',(-13.4161718177499,-16.8660160353187,
21.));
#11391=CARTESIAN_POINT('Ctrl Pts',(-13.4243062623592,-16.9170380509036,
0.));
#11392=CARTESIAN_POINT('Ctrl Pts',(-13.4243062623592,-16.9170380509036,
21.));
#11393=CARTESIAN_POINT('Ctrl Pts',(-13.432203941793,-16.9681720567298,0.));
#11394=CARTESIAN_POINT('Ctrl Pts',(-13.432203941793,-16.9681720567298,21.));
#11395=CARTESIAN_POINT('Ctrl Pts',(-13.4398657451291,-17.0194162803447,
0.));
#11396=CARTESIAN_POINT('Ctrl Pts',(-13.4398657451291,-17.0194162803447,
21.));
#11397=CARTESIAN_POINT('Ctrl Pts',(-13.4472925380889,-17.0707690194411,
0.));
#11398=CARTESIAN_POINT('Ctrl Pts',(-13.4472925380889,-17.0707690194411,
21.));
#11399=CARTESIAN_POINT('Ctrl Pts',(-13.4544851484583,-17.1222287365697,
0.));
#11400=CARTESIAN_POINT('Ctrl Pts',(-13.4544851484583,-17.1222287365697,
21.));
#11401=CARTESIAN_POINT('Ctrl Pts',(-13.4614443545811,-17.1737941556239,
0.));
#11402=CARTESIAN_POINT('Ctrl Pts',(-13.4614443545811,-17.1737941556239,
21.));
#11403=CARTESIAN_POINT('Ctrl Pts',(-13.4681708717969,-17.2254643437923,
0.));
#11404=CARTESIAN_POINT('Ctrl Pts',(-13.4681708717969,-17.2254643437923,
21.));
#11405=CARTESIAN_POINT('Ctrl Pts',(-13.474665315482,-17.2772386565028,0.));
#11406=CARTESIAN_POINT('Ctrl Pts',(-13.474665315482,-17.2772386565028,21.));
#11407=CARTESIAN_POINT('Ctrl Pts',(-13.4796755969465,-17.3187410868027,
0.));
#11408=CARTESIAN_POINT('Ctrl Pts',(-13.4796755969465,-17.3187410868027,
21.));
#11409=CARTESIAN_POINT('Ctrl Pts',(-13.4833292332349,-17.3499144948292,
0.));
#11410=CARTESIAN_POINT('Ctrl Pts',(-13.4833292332349,-17.3499144948292,
21.));
#11411=CARTESIAN_POINT('Ctrl Pts',(-13.485718750657,-17.3707174645609,0.));
#11412=CARTESIAN_POINT('Ctrl Pts',(-13.485718750657,-17.3707174645609,21.));
#11413=CARTESIAN_POINT('Ctrl Pts',(-13.4869019493419,-17.3811241238545,
0.));
#11414=CARTESIAN_POINT('Ctrl Pts',(-13.4869019493419,-17.3811241238545,
21.));
#11415=CARTESIAN_POINT('Ctrl Pts',(-12.4172651441477,-14.1074595503134,
0.));
#11416=CARTESIAN_POINT('Ctrl Pts',(-12.4234926340671,-14.1145347042316,
0.));
#11417=CARTESIAN_POINT('Ctrl Pts',(-12.4357509724316,-14.1288394445866,
0.));
#11418=CARTESIAN_POINT('Ctrl Pts',(-12.4535485619996,-14.1507598477672,
0.));
#11419=CARTESIAN_POINT('Ctrl Pts',(-12.4761570639125,-14.1808688343892,
0.));
#11420=CARTESIAN_POINT('Ctrl Pts',(-12.5028859651751,-14.2197144660135,
0.));
#11421=CARTESIAN_POINT('Ctrl Pts',(-12.5285125321527,-14.2594378207584,
0.));
#11422=CARTESIAN_POINT('Ctrl Pts',(-12.5534605602317,-14.2997103098726,
0.));
#11423=CARTESIAN_POINT('Ctrl Pts',(-12.5780443898087,-14.3402859058353,
0.));
#11424=CARTESIAN_POINT('Ctrl Pts',(-12.6023830189244,-14.3810669346235,
0.));
#11425=CARTESIAN_POINT('Ctrl Pts',(-12.626464614311,-14.4220553460485,0.));
#11426=CARTESIAN_POINT('Ctrl Pts',(-12.6501984687124,-14.463313553928,0.));
#11427=CARTESIAN_POINT('Ctrl Pts',(-12.6734695081852,-14.5049233087958,
0.));
#11428=CARTESIAN_POINT('Ctrl Pts',(-12.6961966430455,-14.5469417071951,
0.));
#11429=CARTESIAN_POINT('Ctrl Pts',(-12.7183743139638,-14.5893698147583,
0.));
#11430=CARTESIAN_POINT('Ctrl Pts',(-12.7400427996251,-14.6321748083434,
0.));
#11431=CARTESIAN_POINT('Ctrl Pts',(-12.7612687078867,-14.6753044633399,
0.));
#11432=CARTESIAN_POINT('Ctrl Pts',(-12.7821227233337,-14.7187037124277,
0.));
#11433=CARTESIAN_POINT('Ctrl Pts',(-12.8026557145457,-14.7623324139791,
0.));
#11434=CARTESIAN_POINT('Ctrl Pts',(-12.8228846016791,-14.8061758577898,
0.));
#11435=CARTESIAN_POINT('Ctrl Pts',(-12.8428057266944,-14.8502347891476,
0.));
#11436=CARTESIAN_POINT('Ctrl Pts',(-12.8624032236317,-14.8945191569251,
0.));
#11437=CARTESIAN_POINT('Ctrl Pts',(-12.8816587472147,-14.9390408507356,
0.));
#11438=CARTESIAN_POINT('Ctrl Pts',(-12.9005620742036,-14.9838057866976,
0.));
#11439=CARTESIAN_POINT('Ctrl Pts',(-12.9191164383568,-15.0288099208306,
0.));
#11440=CARTESIAN_POINT('Ctrl Pts',(-12.9373327960422,-15.0740435169624,
0.));
#11441=CARTESIAN_POINT('Ctrl Pts',(-12.9552263908864,-15.1194937003528,
0.));
#11442=CARTESIAN_POINT('Ctrl Pts',(-12.9728126886697,-15.1651474813659,
0.));
#11443=CARTESIAN_POINT('Ctrl Pts',(-12.9901029059182,-15.2109950816083,
0.));
#11444=CARTESIAN_POINT('Ctrl Pts',(-13.0071020851025,-15.2570313635503,
0.));
#11445=CARTESIAN_POINT('Ctrl Pts',(-13.0238115816728,-15.3032539741328,
0.));
#11446=CARTESIAN_POINT('Ctrl Pts',(-13.0402305665115,-15.3496622219036,
0.));
#11447=CARTESIAN_POINT('Ctrl Pts',(-13.0563577967298,-15.3962557545684,
0.));
#11448=CARTESIAN_POINT('Ctrl Pts',(-13.0721935806302,-15.4430330918328,
0.));
#11449=CARTESIAN_POINT('Ctrl Pts',(-13.087740560189,-15.4899910401523,0.));
#11450=CARTESIAN_POINT('Ctrl Pts',(-13.1030026646917,-15.5371254712111,
0.));
#11451=CARTESIAN_POINT('Ctrl Pts',(-13.1179844917497,-15.5844317820184,
0.));
#11452=CARTESIAN_POINT('Ctrl Pts',(-13.1326905726717,-15.6319054413079,
0.));
#11453=CARTESIAN_POINT('Ctrl Pts',(-13.147124558532,-15.6795425955901,0.));
#11454=CARTESIAN_POINT('Ctrl Pts',(-13.161288914421,-15.7273402954914,0.));
#11455=CARTESIAN_POINT('Ctrl Pts',(-13.1751853728467,-15.7752961549278,
0.));
#11456=CARTESIAN_POINT('Ctrl Pts',(-13.1888152101588,-15.8234081427091,
0.));
#11457=CARTESIAN_POINT('Ctrl Pts',(-13.2021795724682,-15.8716743375555,
0.));
#11458=CARTESIAN_POINT('Ctrl Pts',(-13.2152798388134,-15.9200926550954,
0.));
#11459=CARTESIAN_POINT('Ctrl Pts',(-13.2281177675127,-15.9686607385389,
0.));
#11460=CARTESIAN_POINT('Ctrl Pts',(-13.240695304984,-16.0173761036734,0.));
#11461=CARTESIAN_POINT('Ctrl Pts',(-13.2530144750236,-16.0662362238032,
0.));
#11462=CARTESIAN_POINT('Ctrl Pts',(-13.2650772466062,-16.1152386305152,
0.));
#11463=CARTESIAN_POINT('Ctrl Pts',(-13.2768853909882,-16.1643810242643,
0.));
#11464=CARTESIAN_POINT('Ctrl Pts',(-13.2884404210388,-16.2136613184475,
0.));
#11465=CARTESIAN_POINT('Ctrl Pts',(-13.2997436744733,-16.2630775678735,
0.));
#11466=CARTESIAN_POINT('Ctrl Pts',(-13.3107963665229,-16.3126279218067,
0.));
#11467=CARTESIAN_POINT('Ctrl Pts',(-13.3215996524974,-16.3623105703343,
0.));
#11468=CARTESIAN_POINT('Ctrl Pts',(-13.3321546976812,-16.4121236828756,
0.));
#11469=CARTESIAN_POINT('Ctrl Pts',(-13.3424627129921,-16.4620653818862,
0.));
#11470=CARTESIAN_POINT('Ctrl Pts',(-13.3525249163084,-16.5121337902953,
0.));
#11471=CARTESIAN_POINT('Ctrl Pts',(-13.3623425108873,-16.5623270636327,
0.));
#11472=CARTESIAN_POINT('Ctrl Pts',(-13.3719166600676,-16.612643424234,0.));
#11473=CARTESIAN_POINT('Ctrl Pts',(-13.381248462113,-16.6630812012276,0.));
#11474=CARTESIAN_POINT('Ctrl Pts',(-13.3903389370346,-16.7136388432444,
0.));
#11475=CARTESIAN_POINT('Ctrl Pts',(-13.3991890464165,-16.7643148579872,
0.));
#11476=CARTESIAN_POINT('Ctrl Pts',(-13.4077997088426,-16.8151077630226,
0.));
#11477=CARTESIAN_POINT('Ctrl Pts',(-13.4161718177499,-16.8660160353187,
0.));
#11478=CARTESIAN_POINT('Ctrl Pts',(-13.4243062623592,-16.9170380509036,
0.));
#11479=CARTESIAN_POINT('Ctrl Pts',(-13.432203941793,-16.9681720567298,0.));
#11480=CARTESIAN_POINT('Ctrl Pts',(-13.4398657451291,-17.0194162803447,
0.));
#11481=CARTESIAN_POINT('Ctrl Pts',(-13.4472925380889,-17.0707690194411,
0.));
#11482=CARTESIAN_POINT('Ctrl Pts',(-13.4544851484583,-17.1222287365697,
0.));
#11483=CARTESIAN_POINT('Ctrl Pts',(-13.4614443545811,-17.1737941556239,
0.));
#11484=CARTESIAN_POINT('Ctrl Pts',(-13.4695161752401,-17.235798381426,0.));
#11485=CARTESIAN_POINT('Ctrl Pts',(-13.4759526005425,-17.287598725272,0.));
#11486=CARTESIAN_POINT('Ctrl Pts',(-13.4809165957478,-17.3291218739796,
0.));
#11487=CARTESIAN_POINT('Ctrl Pts',(-13.4845355519784,-17.360310805254,0.));
#11488=CARTESIAN_POINT('Ctrl Pts',(-13.4869019493419,-17.3811241238545,
0.));
#11489=CARTESIAN_POINT('Ctrl Pts',(-12.4172651441477,-14.1074595503134,
13.));
#11490=CARTESIAN_POINT('Ctrl Pts',(-12.4277613166149,-14.1193844248164,
13.));
#11491=CARTESIAN_POINT('Ctrl Pts',(-12.4379186757848,-14.1315753314249,
13.));
#11492=CARTESIAN_POINT('Ctrl Pts',(-12.4477599775084,-14.14401474732,13.));
#11493=CARTESIAN_POINT('Ctrl Pts',(-12.45929471922,-14.1585946731696,13.));
#11494=CARTESIAN_POINT('Ctrl Pts',(-12.4703959522577,-14.1735154808295,
13.));
#11495=CARTESIAN_POINT('Ctrl Pts',(-12.4811568677436,-14.1887053040703,
13.));
#11496=CARTESIAN_POINT('Ctrl Pts',(-12.4962979908344,-14.2100781123335,
13.));
#11497=CARTESIAN_POINT('Ctrl Pts',(-12.5107710847127,-14.2319791941756,
13.));
#11498=CARTESIAN_POINT('Ctrl Pts',(-12.5249003586941,-14.254157574695,13.));
#11499=CARTESIAN_POINT('Ctrl Pts',(-12.5342985542355,-14.2689096955178,
13.));
#11500=CARTESIAN_POINT('Ctrl Pts',(-12.5435462296413,-14.2837832480516,
13.));
#11501=CARTESIAN_POINT('Ctrl Pts',(-12.5527146050322,-14.298722508524,13.));
#11502=CARTESIAN_POINT('Ctrl Pts',(-12.5623658230416,-14.3144485290642,
13.));
#11503=CARTESIAN_POINT('Ctrl Pts',(-12.5719298675028,-14.330246820686,13.));
#11504=CARTESIAN_POINT('Ctrl Pts',(-12.5814385821519,-14.3460912752807,
13.));
#11505=CARTESIAN_POINT('Ctrl Pts',(-12.5919985302804,-14.3636874094394,
13.));
#11506=CARTESIAN_POINT('Ctrl Pts',(-12.6024891912727,-14.381341260665,13.));
#11507=CARTESIAN_POINT('Ctrl Pts',(-12.6128991700701,-14.3990589912032,
13.));
#11508=CARTESIAN_POINT('Ctrl Pts',(-12.6285927183677,-14.4257693299403,
13.));
#11509=CARTESIAN_POINT('Ctrl Pts',(-12.6440977931351,-14.452628589856,13.));
#11510=CARTESIAN_POINT('Ctrl Pts',(-12.6592867998067,-14.4797266308813,
13.));
#11511=CARTESIAN_POINT('Ctrl Pts',(-12.6703212810873,-14.4994127652612,
13.));
#11512=CARTESIAN_POINT('Ctrl Pts',(-12.6811863451307,-14.5192269386383,
13.));
#11513=CARTESIAN_POINT('Ctrl Pts',(-12.6918647171384,-14.5391805041508,
13.));
#11514=CARTESIAN_POINT('Ctrl Pts',(-12.7049181125412,-14.5635720293892,
13.));
#11515=CARTESIAN_POINT('Ctrl Pts',(-12.7176935524276,-14.5881710816651,
13.));
#11516=CARTESIAN_POINT('Ctrl Pts',(-12.7302281821981,-14.612947560673,13.));
#11517=CARTESIAN_POINT('Ctrl Pts',(-12.7437676626773,-14.6397102700639,
13.));
#11518=CARTESIAN_POINT('Ctrl Pts',(-12.7570309720221,-14.6666764215902,
13.));
#11519=CARTESIAN_POINT('Ctrl Pts',(-12.7700903554915,-14.6937895363403,
13.));
#11520=CARTESIAN_POINT('Ctrl Pts',(-12.7821467169645,-14.7188202365146,
13.));
#11521=CARTESIAN_POINT('Ctrl Pts',(-12.7940312932614,-14.7439746960234,
13.));
#11522=CARTESIAN_POINT('Ctrl Pts',(-12.8057660290113,-14.7692347187417,
13.));
#11523=CARTESIAN_POINT('Ctrl Pts',(-12.8217082700361,-14.803551756556,13.));
#11524=CARTESIAN_POINT('Ctrl Pts',(-12.8373723698026,-14.8380647951195,
13.));
#11525=CARTESIAN_POINT('Ctrl Pts',(-12.8527323828632,-14.8727890594695,
13.));
#11526=CARTESIAN_POINT('Ctrl Pts',(-12.8675544637349,-14.9062972246235,
13.));
#11527=CARTESIAN_POINT('Ctrl Pts',(-12.8820871276608,-14.9400067536049,
13.));
#11528=CARTESIAN_POINT('Ctrl Pts',(-12.8963159096104,-14.9739251233868,
13.));
#11529=CARTESIAN_POINT('Ctrl Pts',(-12.9156461084266,-15.0200041787641,
13.));
#11530=CARTESIAN_POINT('Ctrl Pts',(-12.9344180544673,-15.0664667162746,
13.));
#11531=CARTESIAN_POINT('Ctrl Pts',(-12.9526968521306,-15.1132567586771,
13.));
#11532=CARTESIAN_POINT('Ctrl Pts',(-12.968763518006,-15.1543841890161,13.));
#11533=CARTESIAN_POINT('Ctrl Pts',(-12.9844546719519,-15.195760575808,13.));
#11534=CARTESIAN_POINT('Ctrl Pts',(-12.9997938464524,-15.2373637638391,
13.));
#11535=CARTESIAN_POINT('Ctrl Pts',(-13.0224075138791,-15.298696963875,13.));
#11536=CARTESIAN_POINT('Ctrl Pts',(-13.0442489122199,-15.3605284720727,
13.));
#11537=CARTESIAN_POINT('Ctrl Pts',(-13.0653151028182,-15.4228468913963,
13.));
#11538=CARTESIAN_POINT('Ctrl Pts',(-13.0919008408175,-15.501493344391,13.));
#11539=CARTESIAN_POINT('Ctrl Pts',(-13.1172560779889,-15.580912148319,13.));
#11540=CARTESIAN_POINT('Ctrl Pts',(-13.1414683121723,-15.6610132193903,
13.));
#11541=CARTESIAN_POINT('Ctrl Pts',(-13.1742656500639,-15.7695162957074,
13.));
#11542=CARTESIAN_POINT('Ctrl Pts',(-13.2049609859192,-15.8792747460898,
13.));
#11543=CARTESIAN_POINT('Ctrl Pts',(-13.2336341230354,-15.9901726544041,
13.));
#11544=CARTESIAN_POINT('Ctrl Pts',(-13.2591969755247,-16.089041043312,13.));
#11545=CARTESIAN_POINT('Ctrl Pts',(-13.2831593506295,-16.1888100042035,
13.));
#11546=CARTESIAN_POINT('Ctrl Pts',(-13.305579935219,-16.2893994149303,13.));
#11547=CARTESIAN_POINT('Ctrl Pts',(-13.3373560692807,-16.4319622721867,
13.));
#11548=CARTESIAN_POINT('Ctrl Pts',(-13.3660302366011,-16.5761757269041,
13.));
#11549=CARTESIAN_POINT('Ctrl Pts',(-13.3917254924233,-16.7218506225541,
13.));
#11550=CARTESIAN_POINT('Ctrl Pts',(-13.4116849587284,-16.8350074321741,
13.));
#11551=CARTESIAN_POINT('Ctrl Pts',(-13.4298451938425,-16.9490507104974,
13.));
#11552=CARTESIAN_POINT('Ctrl Pts',(-13.4462507334689,-17.063896781128,13.));
#11553=CARTESIAN_POINT('Ctrl Pts',(-13.4604427664362,-17.1632473211086,
13.));
#11554=CARTESIAN_POINT('Ctrl Pts',(-13.4733230167208,-17.2631945741556,
13.));
#11555=CARTESIAN_POINT('Ctrl Pts',(-13.4849093843288,-17.363718437608,13.));
#11556=CARTESIAN_POINT('Ctrl Pts',(-13.4855778874423,-17.3695184016672,
13.));
#11557=CARTESIAN_POINT('Ctrl Pts',(-13.4862420757008,-17.3753202971203,
13.));
#11558=CARTESIAN_POINT('Ctrl Pts',(-13.4869019493419,-17.3811241238545,
13.));
#11559=CARTESIAN_POINT('Ctrl Pts',(-17.3811241238545,-13.4869019493419,
0.));
#11560=CARTESIAN_POINT('Ctrl Pts',(-17.3811241238545,-13.4869019493419,
21.));
#11561=CARTESIAN_POINT('Ctrl Pts',(-17.3707174645609,-13.485718750657,0.));
#11562=CARTESIAN_POINT('Ctrl Pts',(-17.3707174645609,-13.485718750657,21.));
#11563=CARTESIAN_POINT('Ctrl Pts',(-17.3499144948292,-13.4833292332349,
0.));
#11564=CARTESIAN_POINT('Ctrl Pts',(-17.3499144948292,-13.4833292332349,
21.));
#11565=CARTESIAN_POINT('Ctrl Pts',(-17.3187410868027,-13.4796755969465,
0.));
#11566=CARTESIAN_POINT('Ctrl Pts',(-17.3187410868027,-13.4796755969465,
21.));
#11567=CARTESIAN_POINT('Ctrl Pts',(-17.2772386565028,-13.474665315482,0.));
#11568=CARTESIAN_POINT('Ctrl Pts',(-17.2772386565028,-13.474665315482,21.));
#11569=CARTESIAN_POINT('Ctrl Pts',(-17.2254643437923,-13.4681708717969,
0.));
#11570=CARTESIAN_POINT('Ctrl Pts',(-17.2254643437923,-13.4681708717969,
21.));
#11571=CARTESIAN_POINT('Ctrl Pts',(-17.173794155624,-13.4614443545811,0.));
#11572=CARTESIAN_POINT('Ctrl Pts',(-17.173794155624,-13.4614443545811,21.));
#11573=CARTESIAN_POINT('Ctrl Pts',(-17.1222287365697,-13.4544851484583,
0.));
#11574=CARTESIAN_POINT('Ctrl Pts',(-17.1222287365697,-13.4544851484583,
21.));
#11575=CARTESIAN_POINT('Ctrl Pts',(-17.0707690194412,-13.4472925380889,
0.));
#11576=CARTESIAN_POINT('Ctrl Pts',(-17.0707690194412,-13.4472925380889,
21.));
#11577=CARTESIAN_POINT('Ctrl Pts',(-17.0194162803447,-13.4398657451291,
0.));
#11578=CARTESIAN_POINT('Ctrl Pts',(-17.0194162803447,-13.4398657451291,
21.));
#11579=CARTESIAN_POINT('Ctrl Pts',(-16.9681720567298,-13.432203941793,0.));
#11580=CARTESIAN_POINT('Ctrl Pts',(-16.9681720567298,-13.432203941793,21.));
#11581=CARTESIAN_POINT('Ctrl Pts',(-16.9170380509036,-13.4243062623592,
0.));
#11582=CARTESIAN_POINT('Ctrl Pts',(-16.9170380509036,-13.4243062623592,
21.));
#11583=CARTESIAN_POINT('Ctrl Pts',(-16.8660160353187,-13.4161718177499,
0.));
#11584=CARTESIAN_POINT('Ctrl Pts',(-16.8660160353187,-13.4161718177499,
21.));
#11585=CARTESIAN_POINT('Ctrl Pts',(-16.8151077630226,-13.4077997088426,
0.));
#11586=CARTESIAN_POINT('Ctrl Pts',(-16.8151077630226,-13.4077997088426,
21.));
#11587=CARTESIAN_POINT('Ctrl Pts',(-16.7643148579873,-13.3991890464165,
0.));
#11588=CARTESIAN_POINT('Ctrl Pts',(-16.7643148579873,-13.3991890464165,
21.));
#11589=CARTESIAN_POINT('Ctrl Pts',(-16.7136388432444,-13.3903389370346,
0.));
#11590=CARTESIAN_POINT('Ctrl Pts',(-16.7136388432444,-13.3903389370346,
21.));
#11591=CARTESIAN_POINT('Ctrl Pts',(-16.6630812012276,-13.381248462113,0.));
#11592=CARTESIAN_POINT('Ctrl Pts',(-16.6630812012276,-13.381248462113,21.));
#11593=CARTESIAN_POINT('Ctrl Pts',(-16.612643424234,-13.3719166600676,0.));
#11594=CARTESIAN_POINT('Ctrl Pts',(-16.612643424234,-13.3719166600676,21.));
#11595=CARTESIAN_POINT('Ctrl Pts',(-16.5623270636327,-13.3623425108873,
0.));
#11596=CARTESIAN_POINT('Ctrl Pts',(-16.5623270636327,-13.3623425108873,
21.));
#11597=CARTESIAN_POINT('Ctrl Pts',(-16.5121337902953,-13.3525249163084,
0.));
#11598=CARTESIAN_POINT('Ctrl Pts',(-16.5121337902953,-13.3525249163084,
21.));
#11599=CARTESIAN_POINT('Ctrl Pts',(-16.4620653818862,-13.3424627129921,
0.));
#11600=CARTESIAN_POINT('Ctrl Pts',(-16.4620653818862,-13.3424627129921,
21.));
#11601=CARTESIAN_POINT('Ctrl Pts',(-16.4121236828756,-13.3321546976812,
0.));
#11602=CARTESIAN_POINT('Ctrl Pts',(-16.4121236828756,-13.3321546976812,
21.));
#11603=CARTESIAN_POINT('Ctrl Pts',(-16.3623105703343,-13.3215996524974,
0.));
#11604=CARTESIAN_POINT('Ctrl Pts',(-16.3623105703343,-13.3215996524974,
21.));
#11605=CARTESIAN_POINT('Ctrl Pts',(-16.3126279218067,-13.3107963665229,
0.));
#11606=CARTESIAN_POINT('Ctrl Pts',(-16.3126279218067,-13.3107963665229,
21.));
#11607=CARTESIAN_POINT('Ctrl Pts',(-16.2630775678735,-13.2997436744733,
0.));
#11608=CARTESIAN_POINT('Ctrl Pts',(-16.2630775678735,-13.2997436744733,
21.));
#11609=CARTESIAN_POINT('Ctrl Pts',(-16.2136613184475,-13.2884404210387,
0.));
#11610=CARTESIAN_POINT('Ctrl Pts',(-16.2136613184475,-13.2884404210387,
21.));
#11611=CARTESIAN_POINT('Ctrl Pts',(-16.1643810242643,-13.2768853909882,
0.));
#11612=CARTESIAN_POINT('Ctrl Pts',(-16.1643810242643,-13.2768853909882,
21.));
#11613=CARTESIAN_POINT('Ctrl Pts',(-16.1152386305152,-13.2650772466062,
0.));
#11614=CARTESIAN_POINT('Ctrl Pts',(-16.1152386305152,-13.2650772466062,
21.));
#11615=CARTESIAN_POINT('Ctrl Pts',(-16.0662362238032,-13.2530144750236,
0.));
#11616=CARTESIAN_POINT('Ctrl Pts',(-16.0662362238032,-13.2530144750236,
21.));
#11617=CARTESIAN_POINT('Ctrl Pts',(-16.0173761036734,-13.240695304984,0.));
#11618=CARTESIAN_POINT('Ctrl Pts',(-16.0173761036734,-13.240695304984,21.));
#11619=CARTESIAN_POINT('Ctrl Pts',(-15.9686607385389,-13.2281177675127,
0.));
#11620=CARTESIAN_POINT('Ctrl Pts',(-15.9686607385389,-13.2281177675127,
21.));
#11621=CARTESIAN_POINT('Ctrl Pts',(-15.9200926550954,-13.2152798388134,
0.));
#11622=CARTESIAN_POINT('Ctrl Pts',(-15.9200926550954,-13.2152798388134,
21.));
#11623=CARTESIAN_POINT('Ctrl Pts',(-15.8716743375555,-13.2021795724682,
0.));
#11624=CARTESIAN_POINT('Ctrl Pts',(-15.8716743375555,-13.2021795724682,
21.));
#11625=CARTESIAN_POINT('Ctrl Pts',(-15.8234081427091,-13.1888152101588,
0.));
#11626=CARTESIAN_POINT('Ctrl Pts',(-15.8234081427091,-13.1888152101588,
21.));
#11627=CARTESIAN_POINT('Ctrl Pts',(-15.7752961549278,-13.1751853728467,
0.));
#11628=CARTESIAN_POINT('Ctrl Pts',(-15.7752961549278,-13.1751853728467,
21.));
#11629=CARTESIAN_POINT('Ctrl Pts',(-15.7273402954914,-13.161288914421,0.));
#11630=CARTESIAN_POINT('Ctrl Pts',(-15.7273402954914,-13.161288914421,21.));
#11631=CARTESIAN_POINT('Ctrl Pts',(-15.6795425955901,-13.147124558532,0.));
#11632=CARTESIAN_POINT('Ctrl Pts',(-15.6795425955901,-13.147124558532,21.));
#11633=CARTESIAN_POINT('Ctrl Pts',(-15.6319054413079,-13.1326905726717,
0.));
#11634=CARTESIAN_POINT('Ctrl Pts',(-15.6319054413079,-13.1326905726717,
21.));
#11635=CARTESIAN_POINT('Ctrl Pts',(-15.5844317820184,-13.1179844917497,
0.));
#11636=CARTESIAN_POINT('Ctrl Pts',(-15.5844317820184,-13.1179844917497,
21.));
#11637=CARTESIAN_POINT('Ctrl Pts',(-15.5371254712111,-13.1030026646917,
0.));
#11638=CARTESIAN_POINT('Ctrl Pts',(-15.5371254712111,-13.1030026646917,
21.));
#11639=CARTESIAN_POINT('Ctrl Pts',(-15.4899910401523,-13.087740560189,0.));
#11640=CARTESIAN_POINT('Ctrl Pts',(-15.4899910401523,-13.087740560189,21.));
#11641=CARTESIAN_POINT('Ctrl Pts',(-15.4430330918328,-13.0721935806302,
0.));
#11642=CARTESIAN_POINT('Ctrl Pts',(-15.4430330918328,-13.0721935806302,
21.));
#11643=CARTESIAN_POINT('Ctrl Pts',(-15.3962557545684,-13.0563577967298,
0.));
#11644=CARTESIAN_POINT('Ctrl Pts',(-15.3962557545684,-13.0563577967298,
21.));
#11645=CARTESIAN_POINT('Ctrl Pts',(-15.3496622219036,-13.0402305665115,
0.));
#11646=CARTESIAN_POINT('Ctrl Pts',(-15.3496622219036,-13.0402305665115,
21.));
#11647=CARTESIAN_POINT('Ctrl Pts',(-15.3032539741328,-13.0238115816728,
0.));
#11648=CARTESIAN_POINT('Ctrl Pts',(-15.3032539741328,-13.0238115816728,
21.));
#11649=CARTESIAN_POINT('Ctrl Pts',(-15.2570313635503,-13.0071020851025,
0.));
#11650=CARTESIAN_POINT('Ctrl Pts',(-15.2570313635503,-13.0071020851025,
21.));
#11651=CARTESIAN_POINT('Ctrl Pts',(-15.2109950816083,-12.9901029059182,
0.));
#11652=CARTESIAN_POINT('Ctrl Pts',(-15.2109950816083,-12.9901029059182,
21.));
#11653=CARTESIAN_POINT('Ctrl Pts',(-15.1651474813659,-12.9728126886697,
0.));
#11654=CARTESIAN_POINT('Ctrl Pts',(-15.1651474813659,-12.9728126886697,
21.));
#11655=CARTESIAN_POINT('Ctrl Pts',(-15.1194937003528,-12.9552263908864,
0.));
#11656=CARTESIAN_POINT('Ctrl Pts',(-15.1194937003528,-12.9552263908864,
21.));
#11657=CARTESIAN_POINT('Ctrl Pts',(-15.0740435169624,-12.9373327960422,
0.));
#11658=CARTESIAN_POINT('Ctrl Pts',(-15.0740435169624,-12.9373327960422,
21.));
#11659=CARTESIAN_POINT('Ctrl Pts',(-15.0288099208306,-12.9191164383568,
0.));
#11660=CARTESIAN_POINT('Ctrl Pts',(-15.0288099208306,-12.9191164383568,
21.));
#11661=CARTESIAN_POINT('Ctrl Pts',(-14.9838057866976,-12.9005620742036,
0.));
#11662=CARTESIAN_POINT('Ctrl Pts',(-14.9838057866976,-12.9005620742036,
21.));
#11663=CARTESIAN_POINT('Ctrl Pts',(-14.9390408507356,-12.8816587472147,
0.));
#11664=CARTESIAN_POINT('Ctrl Pts',(-14.9390408507356,-12.8816587472147,
21.));
#11665=CARTESIAN_POINT('Ctrl Pts',(-14.8945191569251,-12.8624032236317,
0.));
#11666=CARTESIAN_POINT('Ctrl Pts',(-14.8945191569251,-12.8624032236317,
21.));
#11667=CARTESIAN_POINT('Ctrl Pts',(-14.8502347891476,-12.8428057266944,
0.));
#11668=CARTESIAN_POINT('Ctrl Pts',(-14.8502347891476,-12.8428057266944,
21.));
#11669=CARTESIAN_POINT('Ctrl Pts',(-14.8061758577898,-12.8228846016791,
0.));
#11670=CARTESIAN_POINT('Ctrl Pts',(-14.8061758577898,-12.8228846016791,
21.));
#11671=CARTESIAN_POINT('Ctrl Pts',(-14.7623324139791,-12.8026557145457,
0.));
#11672=CARTESIAN_POINT('Ctrl Pts',(-14.7623324139791,-12.8026557145457,
21.));
#11673=CARTESIAN_POINT('Ctrl Pts',(-14.7187037124277,-12.7821227233337,
0.));
#11674=CARTESIAN_POINT('Ctrl Pts',(-14.7187037124277,-12.7821227233337,
21.));
#11675=CARTESIAN_POINT('Ctrl Pts',(-14.6753044633399,-12.7612687078867,
0.));
#11676=CARTESIAN_POINT('Ctrl Pts',(-14.6753044633399,-12.7612687078867,
21.));
#11677=CARTESIAN_POINT('Ctrl Pts',(-14.6321748083434,-12.7400427996251,
0.));
#11678=CARTESIAN_POINT('Ctrl Pts',(-14.6321748083434,-12.7400427996251,
21.));
#11679=CARTESIAN_POINT('Ctrl Pts',(-14.5893698147583,-12.7183743139638,
0.));
#11680=CARTESIAN_POINT('Ctrl Pts',(-14.5893698147583,-12.7183743139638,
21.));
#11681=CARTESIAN_POINT('Ctrl Pts',(-14.5469417071952,-12.6961966430455,
0.));
#11682=CARTESIAN_POINT('Ctrl Pts',(-14.5469417071952,-12.6961966430455,
21.));
#11683=CARTESIAN_POINT('Ctrl Pts',(-14.5049233087958,-12.6734695081852,
0.));
#11684=CARTESIAN_POINT('Ctrl Pts',(-14.5049233087958,-12.6734695081852,
21.));
#11685=CARTESIAN_POINT('Ctrl Pts',(-14.463313553928,-12.6501984687124,0.));
#11686=CARTESIAN_POINT('Ctrl Pts',(-14.463313553928,-12.6501984687124,21.));
#11687=CARTESIAN_POINT('Ctrl Pts',(-14.4220553460485,-12.626464614311,0.));
#11688=CARTESIAN_POINT('Ctrl Pts',(-14.4220553460485,-12.626464614311,21.));
#11689=CARTESIAN_POINT('Ctrl Pts',(-14.3810669346235,-12.6023830189244,
0.));
#11690=CARTESIAN_POINT('Ctrl Pts',(-14.3810669346235,-12.6023830189244,
21.));
#11691=CARTESIAN_POINT('Ctrl Pts',(-14.3402859058353,-12.5780443898087,
0.));
#11692=CARTESIAN_POINT('Ctrl Pts',(-14.3402859058353,-12.5780443898087,
21.));
#11693=CARTESIAN_POINT('Ctrl Pts',(-14.2997103098726,-12.5534605602317,
0.));
#11694=CARTESIAN_POINT('Ctrl Pts',(-14.2997103098726,-12.5534605602317,
21.));
#11695=CARTESIAN_POINT('Ctrl Pts',(-14.2594378207584,-12.5285125321527,
0.));
#11696=CARTESIAN_POINT('Ctrl Pts',(-14.2594378207584,-12.5285125321527,
21.));
#11697=CARTESIAN_POINT('Ctrl Pts',(-14.2197144660135,-12.502885965175,0.));
#11698=CARTESIAN_POINT('Ctrl Pts',(-14.2197144660135,-12.502885965175,21.));
#11699=CARTESIAN_POINT('Ctrl Pts',(-14.1808688343892,-12.4761570639125,
0.));
#11700=CARTESIAN_POINT('Ctrl Pts',(-14.1808688343892,-12.4761570639125,
21.));
#11701=CARTESIAN_POINT('Ctrl Pts',(-14.1507598477672,-12.4535485619996,
0.));
#11702=CARTESIAN_POINT('Ctrl Pts',(-14.1507598477672,-12.4535485619996,
21.));
#11703=CARTESIAN_POINT('Ctrl Pts',(-14.1288394445866,-12.4357509724316,
0.));
#11704=CARTESIAN_POINT('Ctrl Pts',(-14.1288394445866,-12.4357509724316,
21.));
#11705=CARTESIAN_POINT('Ctrl Pts',(-14.1145347042316,-12.4234926340671,
0.));
#11706=CARTESIAN_POINT('Ctrl Pts',(-14.1145347042316,-12.4234926340671,
21.));
#11707=CARTESIAN_POINT('Ctrl Pts',(-14.1074595503134,-12.4172651441477,
0.));
#11708=CARTESIAN_POINT('Ctrl Pts',(-14.1074595503134,-12.4172651441477,
21.));
#11709=CARTESIAN_POINT('',(-17.3811241238545,-13.486901949342,0.));
#11710=CARTESIAN_POINT('Ctrl Pts',(-14.1074595503134,-12.4172651441477,
0.));
#11711=CARTESIAN_POINT('Ctrl Pts',(-14.1145347042316,-12.4234926340671,
0.));
#11712=CARTESIAN_POINT('Ctrl Pts',(-14.1288394445866,-12.4357509724316,
0.));
#11713=CARTESIAN_POINT('Ctrl Pts',(-14.1507598477672,-12.4535485619996,
0.));
#11714=CARTESIAN_POINT('Ctrl Pts',(-14.1808688343892,-12.4761570639125,
0.));
#11715=CARTESIAN_POINT('Ctrl Pts',(-14.2197144660135,-12.502885965175,0.));
#11716=CARTESIAN_POINT('Ctrl Pts',(-14.2594378207584,-12.5285125321527,
0.));
#11717=CARTESIAN_POINT('Ctrl Pts',(-14.2997103098726,-12.5534605602317,
0.));
#11718=CARTESIAN_POINT('Ctrl Pts',(-14.3402859058353,-12.5780443898087,
0.));
#11719=CARTESIAN_POINT('Ctrl Pts',(-14.3810669346235,-12.6023830189244,
0.));
#11720=CARTESIAN_POINT('Ctrl Pts',(-14.4220553460485,-12.626464614311,0.));
#11721=CARTESIAN_POINT('Ctrl Pts',(-14.463313553928,-12.6501984687124,0.));
#11722=CARTESIAN_POINT('Ctrl Pts',(-14.5049233087958,-12.6734695081852,
0.));
#11723=CARTESIAN_POINT('Ctrl Pts',(-14.5469417071952,-12.6961966430455,
0.));
#11724=CARTESIAN_POINT('Ctrl Pts',(-14.5893698147583,-12.7183743139638,
0.));
#11725=CARTESIAN_POINT('Ctrl Pts',(-14.6321748083434,-12.7400427996251,
0.));
#11726=CARTESIAN_POINT('Ctrl Pts',(-14.6753044633399,-12.7612687078867,
0.));
#11727=CARTESIAN_POINT('Ctrl Pts',(-14.7187037124277,-12.7821227233337,
0.));
#11728=CARTESIAN_POINT('Ctrl Pts',(-14.7623324139791,-12.8026557145457,
0.));
#11729=CARTESIAN_POINT('Ctrl Pts',(-14.8061758577898,-12.8228846016791,
0.));
#11730=CARTESIAN_POINT('Ctrl Pts',(-14.8502347891476,-12.8428057266944,
0.));
#11731=CARTESIAN_POINT('Ctrl Pts',(-14.8945191569251,-12.8624032236317,
0.));
#11732=CARTESIAN_POINT('Ctrl Pts',(-14.9390408507356,-12.8816587472147,
0.));
#11733=CARTESIAN_POINT('Ctrl Pts',(-14.9838057866976,-12.9005620742036,
0.));
#11734=CARTESIAN_POINT('Ctrl Pts',(-15.0288099208306,-12.9191164383568,
0.));
#11735=CARTESIAN_POINT('Ctrl Pts',(-15.0740435169624,-12.9373327960422,
0.));
#11736=CARTESIAN_POINT('Ctrl Pts',(-15.1194937003528,-12.9552263908864,
0.));
#11737=CARTESIAN_POINT('Ctrl Pts',(-15.1651474813659,-12.9728126886697,
0.));
#11738=CARTESIAN_POINT('Ctrl Pts',(-15.2109950816083,-12.9901029059182,
0.));
#11739=CARTESIAN_POINT('Ctrl Pts',(-15.2570313635503,-13.0071020851025,
0.));
#11740=CARTESIAN_POINT('Ctrl Pts',(-15.3032539741328,-13.0238115816728,
0.));
#11741=CARTESIAN_POINT('Ctrl Pts',(-15.3496622219036,-13.0402305665115,
0.));
#11742=CARTESIAN_POINT('Ctrl Pts',(-15.3962557545684,-13.0563577967298,
0.));
#11743=CARTESIAN_POINT('Ctrl Pts',(-15.4430330918328,-13.0721935806302,
0.));
#11744=CARTESIAN_POINT('Ctrl Pts',(-15.4899910401523,-13.087740560189,0.));
#11745=CARTESIAN_POINT('Ctrl Pts',(-15.5371254712111,-13.1030026646917,
0.));
#11746=CARTESIAN_POINT('Ctrl Pts',(-15.5844317820184,-13.1179844917497,
0.));
#11747=CARTESIAN_POINT('Ctrl Pts',(-15.6319054413079,-13.1326905726717,
0.));
#11748=CARTESIAN_POINT('Ctrl Pts',(-15.6795425955901,-13.147124558532,0.));
#11749=CARTESIAN_POINT('Ctrl Pts',(-15.7273402954914,-13.161288914421,0.));
#11750=CARTESIAN_POINT('Ctrl Pts',(-15.7752961549278,-13.1751853728467,
0.));
#11751=CARTESIAN_POINT('Ctrl Pts',(-15.8234081427091,-13.1888152101588,
0.));
#11752=CARTESIAN_POINT('Ctrl Pts',(-15.8716743375555,-13.2021795724682,
0.));
#11753=CARTESIAN_POINT('Ctrl Pts',(-15.9200926550954,-13.2152798388134,
0.));
#11754=CARTESIAN_POINT('Ctrl Pts',(-15.9686607385389,-13.2281177675127,
0.));
#11755=CARTESIAN_POINT('Ctrl Pts',(-16.0173761036734,-13.240695304984,0.));
#11756=CARTESIAN_POINT('Ctrl Pts',(-16.0662362238032,-13.2530144750236,
0.));
#11757=CARTESIAN_POINT('Ctrl Pts',(-16.1152386305152,-13.2650772466062,
0.));
#11758=CARTESIAN_POINT('Ctrl Pts',(-16.1643810242643,-13.2768853909882,
0.));
#11759=CARTESIAN_POINT('Ctrl Pts',(-16.2136613184475,-13.2884404210387,
0.));
#11760=CARTESIAN_POINT('Ctrl Pts',(-16.2630775678735,-13.2997436744733,
0.));
#11761=CARTESIAN_POINT('Ctrl Pts',(-16.3126279218067,-13.3107963665229,
0.));
#11762=CARTESIAN_POINT('Ctrl Pts',(-16.3623105703343,-13.3215996524974,
0.));
#11763=CARTESIAN_POINT('Ctrl Pts',(-16.4121236828756,-13.3321546976812,
0.));
#11764=CARTESIAN_POINT('Ctrl Pts',(-16.4620653818862,-13.3424627129921,
0.));
#11765=CARTESIAN_POINT('Ctrl Pts',(-16.5121337902953,-13.3525249163084,
0.));
#11766=CARTESIAN_POINT('Ctrl Pts',(-16.5623270636327,-13.3623425108873,
0.));
#11767=CARTESIAN_POINT('Ctrl Pts',(-16.612643424234,-13.3719166600676,0.));
#11768=CARTESIAN_POINT('Ctrl Pts',(-16.6630812012276,-13.381248462113,0.));
#11769=CARTESIAN_POINT('Ctrl Pts',(-16.7136388432444,-13.3903389370346,
0.));
#11770=CARTESIAN_POINT('Ctrl Pts',(-16.7643148579873,-13.3991890464165,
0.));
#11771=CARTESIAN_POINT('Ctrl Pts',(-16.8151077630226,-13.4077997088426,
0.));
#11772=CARTESIAN_POINT('Ctrl Pts',(-16.8660160353187,-13.4161718177499,
0.));
#11773=CARTESIAN_POINT('Ctrl Pts',(-16.9170380509036,-13.4243062623592,
0.));
#11774=CARTESIAN_POINT('Ctrl Pts',(-16.9681720567298,-13.432203941793,0.));
#11775=CARTESIAN_POINT('Ctrl Pts',(-17.0194162803447,-13.4398657451291,
0.));
#11776=CARTESIAN_POINT('Ctrl Pts',(-17.0707690194412,-13.4472925380889,
0.));
#11777=CARTESIAN_POINT('Ctrl Pts',(-17.1222287365697,-13.4544851484583,
0.));
#11778=CARTESIAN_POINT('Ctrl Pts',(-17.173794155624,-13.4614443545811,0.));
#11779=CARTESIAN_POINT('Ctrl Pts',(-17.235798381426,-13.4695161752401,0.));
#11780=CARTESIAN_POINT('Ctrl Pts',(-17.287598725272,-13.4759526005425,0.));
#11781=CARTESIAN_POINT('Ctrl Pts',(-17.3291218739796,-13.4809165957478,
0.));
#11782=CARTESIAN_POINT('Ctrl Pts',(-17.360310805254,-13.4845355519784,0.));
#11783=CARTESIAN_POINT('Ctrl Pts',(-17.3811241238545,-13.4869019493419,
0.));
#11784=CARTESIAN_POINT('',(-17.3811241238545,-13.486901949342,13.));
#11785=CARTESIAN_POINT('Ctrl Pts',(-17.3811241238545,-13.4869019493419,
13.));
#11786=CARTESIAN_POINT('Ctrl Pts',(-17.2786694026925,-13.475253226354,13.));
#11787=CARTESIAN_POINT('Ctrl Pts',(-17.1768129075703,-13.4622625504827,
13.));
#11788=CARTESIAN_POINT('Ctrl Pts',(-17.0755735571127,-13.4479123002588,
13.));
#11789=CARTESIAN_POINT('Ctrl Pts',(-16.9078155768783,-13.4241333152838,
13.));
#11790=CARTESIAN_POINT('Ctrl Pts',(-16.7417653304334,-13.3966181281356,
13.));
#11791=CARTESIAN_POINT('Ctrl Pts',(-16.57767452627,-13.365224404591,13.));
#11792=CARTESIAN_POINT('Ctrl Pts',(-16.4515447134285,-13.341093348038,13.));
#11793=CARTESIAN_POINT('Ctrl Pts',(-16.3265706105421,-13.3146689195875,
13.));
#11794=CARTESIAN_POINT('Ctrl Pts',(-16.2028831155019,-13.2858665160047,
13.));
#11795=CARTESIAN_POINT('Ctrl Pts',(-16.06973651931,-13.2548614253288,13.));
#11796=CARTESIAN_POINT('Ctrl Pts',(-15.9380763844413,-13.221105276728,13.));
#11797=CARTESIAN_POINT('Ctrl Pts',(-15.8081115249869,-13.1844379732027,
13.));
#11798=CARTESIAN_POINT('Ctrl Pts',(-15.7361594390004,-13.1641379552808,
13.));
#11799=CARTESIAN_POINT('Ctrl Pts',(-15.6647240119351,-13.1429498666824,
13.));
#11800=CARTESIAN_POINT('Ctrl Pts',(-15.5938437094451,-13.1208442193483,
13.));
#11801=CARTESIAN_POINT('Ctrl Pts',(-15.5255406814322,-13.0995423541465,
13.));
#11802=CARTESIAN_POINT('Ctrl Pts',(-15.4577571787665,-13.0773830005559,
13.));
#11803=CARTESIAN_POINT('Ctrl Pts',(-15.3905488552889,-13.0543129132427,
13.));
#11804=CARTESIAN_POINT('Ctrl Pts',(-15.33246024466,-13.0343732800281,13.));
#11805=CARTESIAN_POINT('Ctrl Pts',(-15.2747993584962,-13.0137559287927,
13.));
#11806=CARTESIAN_POINT('Ctrl Pts',(-15.2175748374047,-12.9924643459712,
13.));
#11807=CARTESIAN_POINT('Ctrl Pts',(-15.1765073882052,-12.9771843404906,
13.));
#11808=CARTESIAN_POINT('Ctrl Pts',(-15.1356630008116,-12.9615593601525,
13.));
#11809=CARTESIAN_POINT('Ctrl Pts',(-15.0950681407047,-12.9455599556256,
13.));
#11810=CARTESIAN_POINT('Ctrl Pts',(-15.0551343157937,-12.9298210808671,
13.));
#11811=CARTESIAN_POINT('Ctrl Pts',(-15.0154457689919,-12.9137147531571,
13.));
#11812=CARTESIAN_POINT('Ctrl Pts',(-14.9760367892541,-12.8972012565818,
13.));
#11813=CARTESIAN_POINT('Ctrl Pts',(-14.9418668889764,-12.8828830850643,
13.));
#11814=CARTESIAN_POINT('Ctrl Pts',(-14.9079086467,-12.8682568220943,13.));
#11815=CARTESIAN_POINT('Ctrl Pts',(-14.8741550424141,-12.853336407922,13.));
#11816=CARTESIAN_POINT('Ctrl Pts',(-14.8435820222663,-12.8398219364233,
13.));
#11817=CARTESIAN_POINT('Ctrl Pts',(-14.8131735649528,-12.8260705988221,
13.));
#11818=CARTESIAN_POINT('Ctrl Pts',(-14.782917409017,-12.8121025758909,13.));
#11819=CARTESIAN_POINT('Ctrl Pts',(-14.7574312210357,-12.8003366510026,
13.));
#11820=CARTESIAN_POINT('Ctrl Pts',(-14.7320520621591,-12.7884183713523,
13.));
#11821=CARTESIAN_POINT('Ctrl Pts',(-14.7067929859341,-12.7763327021684,
13.));
#11822=CARTESIAN_POINT('Ctrl Pts',(-14.6702403530813,-12.7588434232842,
13.));
#11823=CARTESIAN_POINT('Ctrl Pts',(-14.6339396294117,-12.7410029355977,
13.));
#11824=CARTESIAN_POINT('Ctrl Pts',(-14.5980256539368,-12.7226389620173,
13.));
#11825=CARTESIAN_POINT('Ctrl Pts',(-14.5763250375761,-12.7115427372118,
13.));
#11826=CARTESIAN_POINT('Ctrl Pts',(-14.5547677199977,-12.7002526009286,
13.));
#11827=CARTESIAN_POINT('Ctrl Pts',(-14.533370542697,-12.6887481998661,13.));
#11828=CARTESIAN_POINT('Ctrl Pts',(-14.513636325704,-12.6781379056319,13.));
#11829=CARTESIAN_POINT('Ctrl Pts',(-14.494039116296,-12.6673442954742,13.));
#11830=CARTESIAN_POINT('Ctrl Pts',(-14.4745649059699,-12.656388173598,13.));
#11831=CARTESIAN_POINT('Ctrl Pts',(-14.4477761569858,-12.6413169181342,
13.));
#11832=CARTESIAN_POINT('Ctrl Pts',(-14.4212156950323,-12.6259439377184,
13.));
#11833=CARTESIAN_POINT('Ctrl Pts',(-14.3947967980035,-12.610392584142,13.));
#11834=CARTESIAN_POINT('Ctrl Pts',(-14.3780361779186,-12.6005265277046,
13.));
#11835=CARTESIAN_POINT('Ctrl Pts',(-14.3613315561545,-12.5905900370373,
13.));
#11836=CARTESIAN_POINT('Ctrl Pts',(-14.3446791500623,-12.5805908896179,
13.));
#11837=CARTESIAN_POINT('Ctrl Pts',(-14.3297343907096,-12.5716171202366,
13.));
#11838=CARTESIAN_POINT('Ctrl Pts',(-14.3148312513707,-12.5625934694128,
13.));
#11839=CARTESIAN_POINT('Ctrl Pts',(-14.2999916563209,-12.5534931963782,
13.));
#11840=CARTESIAN_POINT('Ctrl Pts',(-14.2843922864836,-12.543926997017,13.));
#11841=CARTESIAN_POINT('Ctrl Pts',(-14.2688630442666,-12.5342762592095,
13.));
#11842=CARTESIAN_POINT('Ctrl Pts',(-14.2534670740361,-12.5244602884878,
13.));
#11843=CARTESIAN_POINT('Ctrl Pts',(-14.2278944013872,-12.5081559827352,
13.));
#11844=CARTESIAN_POINT('Ctrl Pts',(-14.2026946288704,-12.4913891918921,
13.));
#11845=CARTESIAN_POINT('Ctrl Pts',(-14.1782508275765,-12.4736648236058,
13.));
#11846=CARTESIAN_POINT('Ctrl Pts',(-14.1647716456531,-12.4638909761696,
13.));
#11847=CARTESIAN_POINT('Ctrl Pts',(-14.1515231428601,-12.4538248359232,
13.));
#11848=CARTESIAN_POINT('Ctrl Pts',(-14.1385523184119,-12.443405435509,13.));
#11849=CARTESIAN_POINT('Ctrl Pts',(-14.1280012216313,-12.4349297906026,
13.));
#11850=CARTESIAN_POINT('Ctrl Pts',(-14.1176338183099,-12.4262204477521,
13.));
#11851=CARTESIAN_POINT('Ctrl Pts',(-14.1074595503134,-12.4172651441477,
13.));
#11852=CARTESIAN_POINT('',(-17.3811241238545,-13.486901949342,0.));
#11853=CARTESIAN_POINT('Origin',(-4.58435815896522E-12,-3.33073116609659E-12,
0.));
#11854=CARTESIAN_POINT('',(-18.1978687191668,-12.3627494547115,0.));
#11855=CARTESIAN_POINT('Origin',(-4.58435815896522E-12,-3.33073116609659E-12,
0.));
#11856=CARTESIAN_POINT('',(-18.1978687191668,-12.3627494547115,13.));
#11857=CARTESIAN_POINT('Origin',(-4.58435815896522E-12,-3.33073116609659E-12,
13.));
#11858=CARTESIAN_POINT('',(-18.1978687191668,-12.3627494547115,0.));
#11859=CARTESIAN_POINT('Ctrl Pts',(-16.1689656784104,-9.57984538049455,
0.));
#11860=CARTESIAN_POINT('Ctrl Pts',(-16.1689656784104,-9.57984538049455,
21.));
#11861=CARTESIAN_POINT('Ctrl Pts',(-16.1770747160769,-9.58464985151482,
0.));
#11862=CARTESIAN_POINT('Ctrl Pts',(-16.1770747160769,-9.58464985151482,
21.));
#11863=CARTESIAN_POINT('Ctrl Pts',(-16.1931534965272,-9.59446643316596,
0.));
#11864=CARTESIAN_POINT('Ctrl Pts',(-16.1931534965272,-9.59446643316596,
21.));
#11865=CARTESIAN_POINT('Ctrl Pts',(-16.2168537871666,-9.60981421781524,
0.));
#11866=CARTESIAN_POINT('Ctrl Pts',(-16.2168537871666,-9.60981421781524,
21.));
#11867=CARTESIAN_POINT('Ctrl Pts',(-16.2476599387841,-9.63146315443273,
0.));
#11868=CARTESIAN_POINT('Ctrl Pts',(-16.2476599387841,-9.63146315443273,
21.));
#11869=CARTESIAN_POINT('Ctrl Pts',(-16.2850845948324,-9.66014786078746,
0.));
#11870=CARTESIAN_POINT('Ctrl Pts',(-16.2850845948324,-9.66014786078746,
21.));
#11871=CARTESIAN_POINT('Ctrl Pts',(-16.3217321000366,-9.69000797146315,
0.));
#11872=CARTESIAN_POINT('Ctrl Pts',(-16.3217321000366,-9.69000797146315,
21.));
#11873=CARTESIAN_POINT('Ctrl Pts',(-16.3579039682519,-9.72060002001012,
0.));
#11874=CARTESIAN_POINT('Ctrl Pts',(-16.3579039682519,-9.72060002001012,
21.));
#11875=CARTESIAN_POINT('Ctrl Pts',(-16.3938231282759,-9.75159288382684,
0.));
#11876=CARTESIAN_POINT('Ctrl Pts',(-16.3938231282759,-9.75159288382684,
21.));
#11877=CARTESIAN_POINT('Ctrl Pts',(-16.4295725710378,-9.78285689698057,
0.));
#11878=CARTESIAN_POINT('Ctrl Pts',(-16.4295725710378,-9.78285689698057,
21.));
#11879=CARTESIAN_POINT('Ctrl Pts',(-16.4651416449558,-9.81439757053278,
0.));
#11880=CARTESIAN_POINT('Ctrl Pts',(-16.4651416449558,-9.81439757053278,
21.));
#11881=CARTESIAN_POINT('Ctrl Pts',(-16.5004633692332,-9.84630229363521,
0.));
#11882=CARTESIAN_POINT('Ctrl Pts',(-16.5004633692332,-9.84630229363521,
21.));
#11883=CARTESIAN_POINT('Ctrl Pts',(-16.5354535643506,-9.8786843754698,0.));
#11884=CARTESIAN_POINT('Ctrl Pts',(-16.5354535643506,-9.8786843754698,21.));
#11885=CARTESIAN_POINT('Ctrl Pts',(-16.5700527532381,-9.91162317616648,
0.));
#11886=CARTESIAN_POINT('Ctrl Pts',(-16.5700527532381,-9.91162317616648,
21.));
#11887=CARTESIAN_POINT('Ctrl Pts',(-16.6042559779574,-9.9451214271291,0.));
#11888=CARTESIAN_POINT('Ctrl Pts',(-16.6042559779574,-9.9451214271291,21.));
#11889=CARTESIAN_POINT('Ctrl Pts',(-16.6380914029057,-9.97913546489641,
0.));
#11890=CARTESIAN_POINT('Ctrl Pts',(-16.6380914029057,-9.97913546489641,
21.));
#11891=CARTESIAN_POINT('Ctrl Pts',(-16.6716062376277,-10.0135950379525,
0.));
#11892=CARTESIAN_POINT('Ctrl Pts',(-16.6716062376277,-10.0135950379525,
21.));
#11893=CARTESIAN_POINT('Ctrl Pts',(-16.7048506904207,-10.0484259314257,
0.));
#11894=CARTESIAN_POINT('Ctrl Pts',(-16.7048506904207,-10.0484259314257,
21.));
#11895=CARTESIAN_POINT('Ctrl Pts',(-16.7378607357337,-10.0835742491038,
0.));
#11896=CARTESIAN_POINT('Ctrl Pts',(-16.7378607357337,-10.0835742491038,
21.));
#11897=CARTESIAN_POINT('Ctrl Pts',(-16.7706479198888,-10.1190207721353,
0.));
#11898=CARTESIAN_POINT('Ctrl Pts',(-16.7706479198888,-10.1190207721353,
21.));
#11899=CARTESIAN_POINT('Ctrl Pts',(-16.8032089941901,-10.1547673397274,
0.));
#11900=CARTESIAN_POINT('Ctrl Pts',(-16.8032089941901,-10.1547673397274,
21.));
#11901=CARTESIAN_POINT('Ctrl Pts',(-16.8355319435838,-10.1908283166713,
0.));
#11902=CARTESIAN_POINT('Ctrl Pts',(-16.8355319435838,-10.1908283166713,
21.));
#11903=CARTESIAN_POINT('Ctrl Pts',(-16.8676029947679,-10.2272206796636,
0.));
#11904=CARTESIAN_POINT('Ctrl Pts',(-16.8676029947679,-10.2272206796636,
21.));
#11905=CARTESIAN_POINT('Ctrl Pts',(-16.8994142530447,-10.2639532144219,
0.));
#11906=CARTESIAN_POINT('Ctrl Pts',(-16.8994142530447,-10.2639532144219,
21.));
#11907=CARTESIAN_POINT('Ctrl Pts',(-16.9309675442426,-10.3010210756062,
0.));
#11908=CARTESIAN_POINT('Ctrl Pts',(-16.9309675442426,-10.3010210756062,
21.));
#11909=CARTESIAN_POINT('Ctrl Pts',(-16.9622702798438,-10.3384116178624,
0.));
#11910=CARTESIAN_POINT('Ctrl Pts',(-16.9622702798438,-10.3384116178624,
21.));
#11911=CARTESIAN_POINT('Ctrl Pts',(-16.9933329788855,-10.3761078860454,
0.));
#11912=CARTESIAN_POINT('Ctrl Pts',(-16.9933329788855,-10.3761078860454,
21.));
#11913=CARTESIAN_POINT('Ctrl Pts',(-17.0241663361802,-10.4140927470882,
0.));
#11914=CARTESIAN_POINT('Ctrl Pts',(-17.0241663361802,-10.4140927470882,
21.));
#11915=CARTESIAN_POINT('Ctrl Pts',(-17.0547779975888,-10.452353435089,0.));
#11916=CARTESIAN_POINT('Ctrl Pts',(-17.0547779975888,-10.452353435089,21.));
#11917=CARTESIAN_POINT('Ctrl Pts',(-17.0851711712016,-10.4908835057575,
0.));
#11918=CARTESIAN_POINT('Ctrl Pts',(-17.0851711712016,-10.4908835057575,
21.));
#11919=CARTESIAN_POINT('Ctrl Pts',(-17.1153464189932,-10.5296803023445,
0.));
#11920=CARTESIAN_POINT('Ctrl Pts',(-17.1153464189932,-10.5296803023445,
21.));
#11921=CARTESIAN_POINT('Ctrl Pts',(-17.1453027387554,-10.5687434234512,
0.));
#11922=CARTESIAN_POINT('Ctrl Pts',(-17.1453027387554,-10.5687434234512,
21.));
#11923=CARTESIAN_POINT('Ctrl Pts',(-17.1750388395657,-10.6080729180997,
0.));
#11924=CARTESIAN_POINT('Ctrl Pts',(-17.1750388395657,-10.6080729180997,
21.));
#11925=CARTESIAN_POINT('Ctrl Pts',(-17.2045545572011,-10.6476672831754,
0.));
#11926=CARTESIAN_POINT('Ctrl Pts',(-17.2045545572011,-10.6476672831754,
21.));
#11927=CARTESIAN_POINT('Ctrl Pts',(-17.2338514174709,-10.6875226650217,
0.));
#11928=CARTESIAN_POINT('Ctrl Pts',(-17.2338514174709,-10.6875226650217,
21.));
#11929=CARTESIAN_POINT('Ctrl Pts',(-17.2629318816279,-10.7276339231608,
0.));
#11930=CARTESIAN_POINT('Ctrl Pts',(-17.2629318816279,-10.7276339231608,
21.));
#11931=CARTESIAN_POINT('Ctrl Pts',(-17.2917988998581,-10.7679952591482,
0.));
#11932=CARTESIAN_POINT('Ctrl Pts',(-17.2917988998581,-10.7679952591482,
21.));
#11933=CARTESIAN_POINT('Ctrl Pts',(-17.3204553814537,-10.8086009632423,
0.));
#11934=CARTESIAN_POINT('Ctrl Pts',(-17.3204553814537,-10.8086009632423,
21.));
#11935=CARTESIAN_POINT('Ctrl Pts',(-17.3489036079991,-10.8494462423128,
0.));
#11936=CARTESIAN_POINT('Ctrl Pts',(-17.3489036079991,-10.8494462423128,
21.));
#11937=CARTESIAN_POINT('Ctrl Pts',(-17.377145012528,-10.8905275295837,0.));
#11938=CARTESIAN_POINT('Ctrl Pts',(-17.377145012528,-10.8905275295837,21.));
#11939=CARTESIAN_POINT('Ctrl Pts',(-17.405180505413,-10.9318420203801,0.));
#11940=CARTESIAN_POINT('Ctrl Pts',(-17.405180505413,-10.9318420203801,21.));
#11941=CARTESIAN_POINT('Ctrl Pts',(-17.4330106728622,-10.9733873885115,
0.));
#11942=CARTESIAN_POINT('Ctrl Pts',(-17.4330106728622,-10.9733873885115,
21.));
#11943=CARTESIAN_POINT('Ctrl Pts',(-17.460636011184,-11.0151614525642,0.));
#11944=CARTESIAN_POINT('Ctrl Pts',(-17.460636011184,-11.0151614525642,21.));
#11945=CARTESIAN_POINT('Ctrl Pts',(-17.4880571878157,-11.0571618040371,
0.));
#11946=CARTESIAN_POINT('Ctrl Pts',(-17.4880571878157,-11.0571618040371,
21.));
#11947=CARTESIAN_POINT('Ctrl Pts',(-17.5152751467292,-11.0993856581394,
0.));
#11948=CARTESIAN_POINT('Ctrl Pts',(-17.5152751467292,-11.0993856581394,
21.));
#11949=CARTESIAN_POINT('Ctrl Pts',(-17.5422909714139,-11.1418300507683,
0.));
#11950=CARTESIAN_POINT('Ctrl Pts',(-17.5422909714139,-11.1418300507683,
21.));
#11951=CARTESIAN_POINT('Ctrl Pts',(-17.5691058058227,-11.1844919535058,
0.));
#11952=CARTESIAN_POINT('Ctrl Pts',(-17.5691058058227,-11.1844919535058,
21.));
#11953=CARTESIAN_POINT('Ctrl Pts',(-17.5957207597803,-11.2273684103051,
0.));
#11954=CARTESIAN_POINT('Ctrl Pts',(-17.5957207597803,-11.2273684103051,
21.));
#11955=CARTESIAN_POINT('Ctrl Pts',(-17.6221368072528,-11.2704566868205,
0.));
#11956=CARTESIAN_POINT('Ctrl Pts',(-17.6221368072528,-11.2704566868205,
21.));
#11957=CARTESIAN_POINT('Ctrl Pts',(-17.6483547422688,-11.3137543310722,
0.));
#11958=CARTESIAN_POINT('Ctrl Pts',(-17.6483547422688,-11.3137543310722,
21.));
#11959=CARTESIAN_POINT('Ctrl Pts',(-17.674375235974,-11.3572590796967,0.));
#11960=CARTESIAN_POINT('Ctrl Pts',(-17.674375235974,-11.3572590796967,21.));
#11961=CARTESIAN_POINT('Ctrl Pts',(-17.700198872213,-11.4009687970126,0.));
#11962=CARTESIAN_POINT('Ctrl Pts',(-17.700198872213,-11.4009687970126,21.));
#11963=CARTESIAN_POINT('Ctrl Pts',(-17.725826190457,-11.4448814046804,0.));
#11964=CARTESIAN_POINT('Ctrl Pts',(-17.725826190457,-11.4448814046804,21.));
#11965=CARTESIAN_POINT('Ctrl Pts',(-17.7512577332768,-11.4889948016216,
0.));
#11966=CARTESIAN_POINT('Ctrl Pts',(-17.7512577332768,-11.4889948016216,
21.));
#11967=CARTESIAN_POINT('Ctrl Pts',(-17.7764940721306,-11.5333068279911,
0.));
#11968=CARTESIAN_POINT('Ctrl Pts',(-17.7764940721306,-11.5333068279911,
21.));
#11969=CARTESIAN_POINT('Ctrl Pts',(-17.8015357852426,-11.5778153222435,
0.));
#11970=CARTESIAN_POINT('Ctrl Pts',(-17.8015357852426,-11.5778153222435,
21.));
#11971=CARTESIAN_POINT('Ctrl Pts',(-17.8263834470057,-11.6225181583564,
0.));
#11972=CARTESIAN_POINT('Ctrl Pts',(-17.8263834470057,-11.6225181583564,
21.));
#11973=CARTESIAN_POINT('Ctrl Pts',(-17.8510376144926,-11.6674132861792,
0.));
#11974=CARTESIAN_POINT('Ctrl Pts',(-17.8510376144926,-11.6674132861792,
21.));
#11975=CARTESIAN_POINT('Ctrl Pts',(-17.8754988158862,-11.7124987772363,
0.));
#11976=CARTESIAN_POINT('Ctrl Pts',(-17.8754988158862,-11.7124987772363,
21.));
#11977=CARTESIAN_POINT('Ctrl Pts',(-17.8997675418752,-11.7577728408871,
0.));
#11978=CARTESIAN_POINT('Ctrl Pts',(-17.8997675418752,-11.7577728408871,
21.));
#11979=CARTESIAN_POINT('Ctrl Pts',(-17.9238442458356,-11.8032337607271,
0.));
#11980=CARTESIAN_POINT('Ctrl Pts',(-17.9238442458356,-11.8032337607271,
21.));
#11981=CARTESIAN_POINT('Ctrl Pts',(-17.9477293432951,-11.8488798430201,
0.));
#11982=CARTESIAN_POINT('Ctrl Pts',(-17.9477293432951,-11.8488798430201,
21.));
#11983=CARTESIAN_POINT('Ctrl Pts',(-17.9714232133203,-11.8947093631895,
0.));
#11984=CARTESIAN_POINT('Ctrl Pts',(-17.9714232133203,-11.8947093631895,
21.));
#11985=CARTESIAN_POINT('Ctrl Pts',(-17.9949261997754,-11.9407205019619,
0.));
#11986=CARTESIAN_POINT('Ctrl Pts',(-17.9949261997754,-11.9407205019619,
21.));
#11987=CARTESIAN_POINT('Ctrl Pts',(-18.0182386160553,-11.986911314246,0.));
#11988=CARTESIAN_POINT('Ctrl Pts',(-18.0182386160553,-11.986911314246,21.));
#11989=CARTESIAN_POINT('Ctrl Pts',(-18.0413607600052,-12.0332798395991,
0.));
#11990=CARTESIAN_POINT('Ctrl Pts',(-18.0413607600052,-12.0332798395991,
21.));
#11991=CARTESIAN_POINT('Ctrl Pts',(-18.0642929289333,-12.0798241915081,
0.));
#11992=CARTESIAN_POINT('Ctrl Pts',(-18.0642929289333,-12.0798241915081,
21.));
#11993=CARTESIAN_POINT('Ctrl Pts',(-18.0870354350128,-12.1265426519718,
0.));
#11994=CARTESIAN_POINT('Ctrl Pts',(-18.0870354350128,-12.1265426519718,
21.));
#11995=CARTESIAN_POINT('Ctrl Pts',(-18.109588624154,-12.1734337668195,0.));
#11996=CARTESIAN_POINT('Ctrl Pts',(-18.109588624154,-12.1734337668195,21.));
#11997=CARTESIAN_POINT('Ctrl Pts',(-18.1319528884305,-12.2204964278426,
0.));
#11998=CARTESIAN_POINT('Ctrl Pts',(-18.1319528884305,-12.2204964278426,
21.));
#11999=CARTESIAN_POINT('Ctrl Pts',(-18.1541286139166,-12.2677298318549,
0.));
#12000=CARTESIAN_POINT('Ctrl Pts',(-18.1541286139166,-12.2677298318549,
21.));
#12001=CARTESIAN_POINT('Ctrl Pts',(-18.1717186310224,-12.3056527265146,
0.));
#12002=CARTESIAN_POINT('Ctrl Pts',(-18.1717186310224,-12.3056527265146,
21.));
#12003=CARTESIAN_POINT('Ctrl Pts',(-18.1848265584754,-12.3341713636489,
0.));
#12004=CARTESIAN_POINT('Ctrl Pts',(-18.1848265584754,-12.3341713636489,
21.));
#12005=CARTESIAN_POINT('Ctrl Pts',(-18.1935275957711,-12.3532177620787,
0.));
#12006=CARTESIAN_POINT('Ctrl Pts',(-18.1935275957711,-12.3532177620787,
21.));
#12007=CARTESIAN_POINT('Ctrl Pts',(-18.1978687191668,-12.3627494547115,
0.));
#12008=CARTESIAN_POINT('Ctrl Pts',(-18.1978687191668,-12.3627494547115,
21.));
#12009=CARTESIAN_POINT('Ctrl Pts',(-16.1689656784104,-9.57984538049455,
0.));
#12010=CARTESIAN_POINT('Ctrl Pts',(-16.1770747160769,-9.58464985151482,
0.));
#12011=CARTESIAN_POINT('Ctrl Pts',(-16.1931534965272,-9.59446643316596,
0.));
#12012=CARTESIAN_POINT('Ctrl Pts',(-16.2168537871666,-9.60981421781524,
0.));
#12013=CARTESIAN_POINT('Ctrl Pts',(-16.2476599387841,-9.63146315443273,
0.));
#12014=CARTESIAN_POINT('Ctrl Pts',(-16.2850845948324,-9.66014786078746,
0.));
#12015=CARTESIAN_POINT('Ctrl Pts',(-16.3217321000366,-9.69000797146315,
0.));
#12016=CARTESIAN_POINT('Ctrl Pts',(-16.3579039682519,-9.72060002001012,
0.));
#12017=CARTESIAN_POINT('Ctrl Pts',(-16.3938231282759,-9.75159288382684,
0.));
#12018=CARTESIAN_POINT('Ctrl Pts',(-16.4295725710378,-9.78285689698057,
0.));
#12019=CARTESIAN_POINT('Ctrl Pts',(-16.4651416449558,-9.81439757053278,
0.));
#12020=CARTESIAN_POINT('Ctrl Pts',(-16.5004633692332,-9.84630229363521,
0.));
#12021=CARTESIAN_POINT('Ctrl Pts',(-16.5354535643506,-9.8786843754698,0.));
#12022=CARTESIAN_POINT('Ctrl Pts',(-16.5700527532381,-9.91162317616648,
0.));
#12023=CARTESIAN_POINT('Ctrl Pts',(-16.6042559779574,-9.9451214271291,0.));
#12024=CARTESIAN_POINT('Ctrl Pts',(-16.6380914029057,-9.97913546489641,
0.));
#12025=CARTESIAN_POINT('Ctrl Pts',(-16.6716062376277,-10.0135950379525,
0.));
#12026=CARTESIAN_POINT('Ctrl Pts',(-16.7048506904207,-10.0484259314257,
0.));
#12027=CARTESIAN_POINT('Ctrl Pts',(-16.7378607357337,-10.0835742491038,
0.));
#12028=CARTESIAN_POINT('Ctrl Pts',(-16.7706479198888,-10.1190207721353,
0.));
#12029=CARTESIAN_POINT('Ctrl Pts',(-16.8032089941901,-10.1547673397274,
0.));
#12030=CARTESIAN_POINT('Ctrl Pts',(-16.8355319435838,-10.1908283166713,
0.));
#12031=CARTESIAN_POINT('Ctrl Pts',(-16.8676029947679,-10.2272206796636,
0.));
#12032=CARTESIAN_POINT('Ctrl Pts',(-16.8994142530447,-10.2639532144219,
0.));
#12033=CARTESIAN_POINT('Ctrl Pts',(-16.9309675442426,-10.3010210756062,
0.));
#12034=CARTESIAN_POINT('Ctrl Pts',(-16.9622702798438,-10.3384116178624,
0.));
#12035=CARTESIAN_POINT('Ctrl Pts',(-16.9933329788855,-10.3761078860454,
0.));
#12036=CARTESIAN_POINT('Ctrl Pts',(-17.0241663361802,-10.4140927470882,
0.));
#12037=CARTESIAN_POINT('Ctrl Pts',(-17.0547779975888,-10.452353435089,0.));
#12038=CARTESIAN_POINT('Ctrl Pts',(-17.0851711712016,-10.4908835057575,
0.));
#12039=CARTESIAN_POINT('Ctrl Pts',(-17.1153464189932,-10.5296803023445,
0.));
#12040=CARTESIAN_POINT('Ctrl Pts',(-17.1453027387554,-10.5687434234512,
0.));
#12041=CARTESIAN_POINT('Ctrl Pts',(-17.1750388395657,-10.6080729180997,
0.));
#12042=CARTESIAN_POINT('Ctrl Pts',(-17.2045545572011,-10.6476672831754,
0.));
#12043=CARTESIAN_POINT('Ctrl Pts',(-17.2338514174709,-10.6875226650217,
0.));
#12044=CARTESIAN_POINT('Ctrl Pts',(-17.2629318816279,-10.7276339231608,
0.));
#12045=CARTESIAN_POINT('Ctrl Pts',(-17.2917988998581,-10.7679952591482,
0.));
#12046=CARTESIAN_POINT('Ctrl Pts',(-17.3204553814537,-10.8086009632423,
0.));
#12047=CARTESIAN_POINT('Ctrl Pts',(-17.3489036079991,-10.8494462423128,
0.));
#12048=CARTESIAN_POINT('Ctrl Pts',(-17.377145012528,-10.8905275295837,0.));
#12049=CARTESIAN_POINT('Ctrl Pts',(-17.405180505413,-10.9318420203801,0.));
#12050=CARTESIAN_POINT('Ctrl Pts',(-17.4330106728622,-10.9733873885115,
0.));
#12051=CARTESIAN_POINT('Ctrl Pts',(-17.460636011184,-11.0151614525642,0.));
#12052=CARTESIAN_POINT('Ctrl Pts',(-17.4880571878157,-11.0571618040371,
0.));
#12053=CARTESIAN_POINT('Ctrl Pts',(-17.5152751467292,-11.0993856581394,
0.));
#12054=CARTESIAN_POINT('Ctrl Pts',(-17.5422909714139,-11.1418300507683,
0.));
#12055=CARTESIAN_POINT('Ctrl Pts',(-17.5691058058227,-11.1844919535058,
0.));
#12056=CARTESIAN_POINT('Ctrl Pts',(-17.5957207597803,-11.2273684103051,
0.));
#12057=CARTESIAN_POINT('Ctrl Pts',(-17.6221368072528,-11.2704566868205,
0.));
#12058=CARTESIAN_POINT('Ctrl Pts',(-17.6483547422688,-11.3137543310722,
0.));
#12059=CARTESIAN_POINT('Ctrl Pts',(-17.674375235974,-11.3572590796967,0.));
#12060=CARTESIAN_POINT('Ctrl Pts',(-17.700198872213,-11.4009687970126,0.));
#12061=CARTESIAN_POINT('Ctrl Pts',(-17.725826190457,-11.4448814046804,0.));
#12062=CARTESIAN_POINT('Ctrl Pts',(-17.7512577332768,-11.4889948016216,
0.));
#12063=CARTESIAN_POINT('Ctrl Pts',(-17.7764940721306,-11.5333068279911,
0.));
#12064=CARTESIAN_POINT('Ctrl Pts',(-17.8015357852426,-11.5778153222435,
0.));
#12065=CARTESIAN_POINT('Ctrl Pts',(-17.8263834470057,-11.6225181583564,
0.));
#12066=CARTESIAN_POINT('Ctrl Pts',(-17.8510376144926,-11.6674132861792,
0.));
#12067=CARTESIAN_POINT('Ctrl Pts',(-17.8754988158862,-11.7124987772363,
0.));
#12068=CARTESIAN_POINT('Ctrl Pts',(-17.8997675418752,-11.7577728408871,
0.));
#12069=CARTESIAN_POINT('Ctrl Pts',(-17.9238442458356,-11.8032337607271,
0.));
#12070=CARTESIAN_POINT('Ctrl Pts',(-17.9477293432951,-11.8488798430201,
0.));
#12071=CARTESIAN_POINT('Ctrl Pts',(-17.9714232133203,-11.8947093631895,
0.));
#12072=CARTESIAN_POINT('Ctrl Pts',(-17.9949261997754,-11.9407205019619,
0.));
#12073=CARTESIAN_POINT('Ctrl Pts',(-18.0182386160553,-11.986911314246,0.));
#12074=CARTESIAN_POINT('Ctrl Pts',(-18.0413607600052,-12.0332798395991,
0.));
#12075=CARTESIAN_POINT('Ctrl Pts',(-18.0642929289333,-12.0798241915081,
0.));
#12076=CARTESIAN_POINT('Ctrl Pts',(-18.0870354350128,-12.1265426519718,
0.));
#12077=CARTESIAN_POINT('Ctrl Pts',(-18.109588624154,-12.1734337668195,0.));
#12078=CARTESIAN_POINT('Ctrl Pts',(-18.1364257412858,-12.2299089600472,
0.));
#12079=CARTESIAN_POINT('Ctrl Pts',(-18.1585543320743,-12.2771850498068,
0.));
#12080=CARTESIAN_POINT('Ctrl Pts',(-18.1761067306718,-12.3151419520839,
0.));
#12081=CARTESIAN_POINT('Ctrl Pts',(-18.1891864723772,-12.3436860694314,
0.));
#12082=CARTESIAN_POINT('Ctrl Pts',(-18.1978687191668,-12.3627494547115,
0.));
#12083=CARTESIAN_POINT('Ctrl Pts',(-16.1689656784104,-9.57984538049455,
13.));
#12084=CARTESIAN_POINT('Ctrl Pts',(-16.1826331205334,-9.58794311444298,
13.));
#12085=CARTESIAN_POINT('Ctrl Pts',(-16.1960605405031,-9.59639855902712,
13.));
#12086=CARTESIAN_POINT('Ctrl Pts',(-16.209264165571,-9.60518801711085,13.));
#12087=CARTESIAN_POINT('Ctrl Pts',(-16.224739801703,-9.6154899193841,13.));
#12088=CARTESIAN_POINT('Ctrl Pts',(-16.2399084848584,-9.62624998107167,
13.));
#12089=CARTESIAN_POINT('Ctrl Pts',(-16.254836637175,-9.63737105568732,13.));
#12090=CARTESIAN_POINT('Ctrl Pts',(-16.2758412618972,-9.65301893989002,
13.));
#12091=CARTESIAN_POINT('Ctrl Pts',(-16.296373798599,-9.66937567449949,13.));
#12092=CARTESIAN_POINT('Ctrl Pts',(-16.3166650331518,-9.68610238201322,
13.));
#12093=CARTESIAN_POINT('Ctrl Pts',(-16.3301619042985,-9.69722828051063,
13.));
#12094=CARTESIAN_POINT('Ctrl Pts',(-16.3435531467518,-9.70851618070807,
13.));
#12095=CARTESIAN_POINT('Ctrl Pts',(-16.3568892752788,-9.7198910779208,13.));
#12096=CARTESIAN_POINT('Ctrl Pts',(-16.3709277366574,-9.73186502184932,
13.));
#12097=CARTESIAN_POINT('Ctrl Pts',(-16.3849056240572,-9.74393463776872,
13.));
#12098=CARTESIAN_POINT('Ctrl Pts',(-16.3988451548219,-9.75606525513648,
13.));
#12099=CARTESIAN_POINT('Ctrl Pts',(-16.414325766791,-9.76953696975778,13.));
#12100=CARTESIAN_POINT('Ctrl Pts',(-16.4297583183324,-9.78308498747417,
13.));
#12101=CARTESIAN_POINT('Ctrl Pts',(-16.4451338763398,-9.79671869019648,
13.));
#12102=CARTESIAN_POINT('Ctrl Pts',(-16.4683132763075,-9.8172721587789,13.));
#12103=CARTESIAN_POINT('Ctrl Pts',(-16.4913594464712,-9.83802550134249,
13.));
#12104=CARTESIAN_POINT('Ctrl Pts',(-16.5141788054336,-9.85910360864921,
13.));
#12105=CARTESIAN_POINT('Ctrl Pts',(-16.5307565708362,-9.87441639279172,
13.));
#12106=CARTESIAN_POINT('Ctrl Pts',(-16.5472127770975,-9.88990330206224,
13.));
#12107=CARTESIAN_POINT('Ctrl Pts',(-16.5635345032205,-9.90558047214324,
13.));
#12108=CARTESIAN_POINT('Ctrl Pts',(-16.5834864158081,-9.92474447016175,
13.));
#12109=CARTESIAN_POINT('Ctrl Pts',(-16.6032381063718,-9.9441917311001,13.));
#12110=CARTESIAN_POINT('Ctrl Pts',(-16.6228156007807,-9.96388214930656,
13.));
#12111=CARTESIAN_POINT('Ctrl Pts',(-16.6439625439398,-9.9851510689085,13.));
#12112=CARTESIAN_POINT('Ctrl Pts',(-16.6649096998191,-10.006698815053,13.));
#12113=CARTESIAN_POINT('Ctrl Pts',(-16.6857083247995,-10.0284493480904,
13.));
#12114=CARTESIAN_POINT('Ctrl Pts',(-16.7049095176705,-10.0485293380076,
13.));
#12115=CARTESIAN_POINT('Ctrl Pts',(-16.7239855768682,-10.0687801145851,
13.));
#12116=CARTESIAN_POINT('Ctrl Pts',(-16.7429517500628,-10.0891775910162,
13.));
#12117=CARTESIAN_POINT('Ctrl Pts',(-16.7687182701337,-10.1168886100216,
13.));
#12118=CARTESIAN_POINT('Ctrl Pts',(-16.7942808297111,-10.1448719871919,
13.));
#12119=CARTESIAN_POINT('Ctrl Pts',(-16.8196194580034,-10.1731502199822,
13.));
#12120=CARTESIAN_POINT('Ctrl Pts',(-16.844070687064,-10.2004381038963,13.));
#12121=CARTESIAN_POINT('Ctrl Pts',(-16.8683088890975,-10.2280069309447,
13.));
#12122=CARTESIAN_POINT('Ctrl Pts',(-16.8923226175541,-10.2558682820918,
13.));
#12123=CARTESIAN_POINT('Ctrl Pts',(-16.9249459403096,-10.2937187080479,
13.));
#12124=CARTESIAN_POINT('Ctrl Pts',(-16.9571568356211,-10.3321063567812,
13.));
#12125=CARTESIAN_POINT('Ctrl Pts',(-16.9889999235317,-10.3709578724058,
13.));
#12126=CARTESIAN_POINT('Ctrl Pts',(-17.0169893055707,-10.4051075100498,
13.));
#12127=CARTESIAN_POINT('Ctrl Pts',(-17.04469848632,-10.4396099589146,13.));
#12128=CARTESIAN_POINT('Ctrl Pts',(-17.0721430001642,-10.474436876203,13.));
#12129=CARTESIAN_POINT('Ctrl Pts',(-17.112602877017,-10.5257802081583,13.));
#12130=CARTESIAN_POINT('Ctrl Pts',(-17.1524822680152,-10.5778361036082,
13.));
#12131=CARTESIAN_POINT('Ctrl Pts',(-17.1917748564523,-10.6305946314222,
13.));
#12132=CARTESIAN_POINT('Ctrl Pts',(-17.2413624862848,-10.6971764080832,
13.));
#12133=CARTESIAN_POINT('Ctrl Pts',(-17.2900185098528,-10.7648729797973,
13.));
#12134=CARTESIAN_POINT('Ctrl Pts',(-17.3377983051247,-10.8335716334697,
13.));
#12135=CARTESIAN_POINT('Ctrl Pts',(-17.4025197212104,-10.9266292559136,
13.));
#12136=CARTESIAN_POINT('Ctrl Pts',(-17.465629946501,-11.0215303643735,13.));
#12137=CARTESIAN_POINT('Ctrl Pts',(-17.5271690583862,-11.1181400554829,
13.));
#12138=CARTESIAN_POINT('Ctrl Pts',(-17.5820327885162,-11.2042701255893,
13.));
#12139=CARTESIAN_POINT('Ctrl Pts',(-17.6356526662346,-11.2917512652755,
13.));
#12140=CARTESIAN_POINT('Ctrl Pts',(-17.6880597469658,-11.3804891386083,
13.));
#12141=CARTESIAN_POINT('Ctrl Pts',(-17.7623349917623,-11.5062551071101,
13.));
#12142=CARTESIAN_POINT('Ctrl Pts',(-17.8341701535583,-11.6345494475067,
13.));
#12143=CARTESIAN_POINT('Ctrl Pts',(-17.9036238122623,-11.7651542350891,
13.));
#12144=CARTESIAN_POINT('Ctrl Pts',(-17.9575737615728,-11.8666049261148,
13.));
#12145=CARTESIAN_POINT('Ctrl Pts',(-18.0100864746768,-11.9694546915569,
13.));
#12146=CARTESIAN_POINT('Ctrl Pts',(-18.0611784501095,-12.0736101881878,
13.));
#12147=CARTESIAN_POINT('Ctrl Pts',(-18.1053768649439,-12.163712553743,13.));
#12148=CARTESIAN_POINT('Ctrl Pts',(-18.1485120955669,-12.2547877895871,
13.));
#12149=CARTESIAN_POINT('Ctrl Pts',(-18.1905949538241,-12.346811245556,13.));
#12150=CARTESIAN_POINT('Ctrl Pts',(-18.1930230491134,-12.3521208117116,
13.));
#12151=CARTESIAN_POINT('Ctrl Pts',(-18.1954476374973,-12.357433548157,13.));
#12152=CARTESIAN_POINT('Ctrl Pts',(-18.1978687191668,-12.3627494547115,
13.));
#12153=CARTESIAN_POINT('Ctrl Pts',(-20.698113262342,-7.455743247944,0.));
#12154=CARTESIAN_POINT('Ctrl Pts',(-20.698113262342,-7.455743247944,21.));
#12155=CARTESIAN_POINT('Ctrl Pts',(-20.6878503127065,-7.45783379370107,
0.));
#12156=CARTESIAN_POINT('Ctrl Pts',(-20.6878503127065,-7.45783379370107,
21.));
#12157=CARTESIAN_POINT('Ctrl Pts',(-20.6673271112931,-7.46198969876653,
0.));
#12158=CARTESIAN_POINT('Ctrl Pts',(-20.6673271112931,-7.46198969876653,
21.));
#12159=CARTESIAN_POINT('Ctrl Pts',(-20.6365504027501,-7.46814799701905,
0.));
#12160=CARTESIAN_POINT('Ctrl Pts',(-20.6365504027501,-7.46814799701905,
21.));
#12161=CARTESIAN_POINT('Ctrl Pts',(-20.5955309838521,-7.47620789245427,
0.));
#12162=CARTESIAN_POINT('Ctrl Pts',(-20.5955309838521,-7.47620789245427,
21.));
#12163=CARTESIAN_POINT('Ctrl Pts',(-20.5442837929044,-7.48603045196744,
0.));
#12164=CARTESIAN_POINT('Ctrl Pts',(-20.5442837929044,-7.48603045196744,
21.));
#12165=CARTESIAN_POINT('Ctrl Pts',(-20.4930639156161,-7.49560012018405,
0.));
#12166=CARTESIAN_POINT('Ctrl Pts',(-20.4930639156161,-7.49560012018405,
21.));
#12167=CARTESIAN_POINT('Ctrl Pts',(-20.4418717748497,-7.50491611266253,
0.));
#12168=CARTESIAN_POINT('Ctrl Pts',(-20.4418717748497,-7.50491611266253,
21.));
#12169=CARTESIAN_POINT('Ctrl Pts',(-20.3907080367098,-7.51397746081993,
0.));
#12170=CARTESIAN_POINT('Ctrl Pts',(-20.3907080367098,-7.51397746081993,
21.));
#12171=CARTESIAN_POINT('Ctrl Pts',(-20.3395736743243,-7.52278303006887,
0.));
#12172=CARTESIAN_POINT('Ctrl Pts',(-20.3395736743243,-7.52278303006887,
21.));
#12173=CARTESIAN_POINT('Ctrl Pts',(-20.2884698940944,-7.53133155804007,
0.));
#12174=CARTESIAN_POINT('Ctrl Pts',(-20.2884698940944,-7.53133155804007,
21.));
#12175=CARTESIAN_POINT('Ctrl Pts',(-20.2373980474879,-7.53962169534166,
0.));
#12176=CARTESIAN_POINT('Ctrl Pts',(-20.2373980474879,-7.53962169534166,
21.));
#12177=CARTESIAN_POINT('Ctrl Pts',(-20.1863595454674,-7.54765204869254,
0.));
#12178=CARTESIAN_POINT('Ctrl Pts',(-20.1863595454674,-7.54765204869254,
21.));
#12179=CARTESIAN_POINT('Ctrl Pts',(-20.1353557774357,-7.55542122125494,
0.));
#12180=CARTESIAN_POINT('Ctrl Pts',(-20.1353557774357,-7.55542122125494,
21.));
#12181=CARTESIAN_POINT('Ctrl Pts',(-20.0843880130978,-7.5629278654946,0.));
#12182=CARTESIAN_POINT('Ctrl Pts',(-20.0843880130978,-7.5629278654946,21.));
#12183=CARTESIAN_POINT('Ctrl Pts',(-20.0334574248557,-7.57017066105972,
0.));
#12184=CARTESIAN_POINT('Ctrl Pts',(-20.0334574248557,-7.57017066105972,
21.));
#12185=CARTESIAN_POINT('Ctrl Pts',(-19.9825651387294,-7.57714827622806,
0.));
#12186=CARTESIAN_POINT('Ctrl Pts',(-19.9825651387294,-7.57714827622806,
21.));
#12187=CARTESIAN_POINT('Ctrl Pts',(-19.931712276832,-7.58385933533351,0.));
#12188=CARTESIAN_POINT('Ctrl Pts',(-19.931712276832,-7.58385933533351,21.));
#12189=CARTESIAN_POINT('Ctrl Pts',(-19.8808999994024,-7.59030238888852,
0.));
#12190=CARTESIAN_POINT('Ctrl Pts',(-19.8808999994024,-7.59030238888852,
21.));
#12191=CARTESIAN_POINT('Ctrl Pts',(-19.830129556152,-7.59647587605448,0.));
#12192=CARTESIAN_POINT('Ctrl Pts',(-19.830129556152,-7.59647587605448,21.));
#12193=CARTESIAN_POINT('Ctrl Pts',(-19.7794022782484,-7.60237814110186,
0.));
#12194=CARTESIAN_POINT('Ctrl Pts',(-19.7794022782484,-7.60237814110186,
21.));
#12195=CARTESIAN_POINT('Ctrl Pts',(-19.7287195480601,-7.60800746969261,
0.));
#12196=CARTESIAN_POINT('Ctrl Pts',(-19.7287195480601,-7.60800746969261,
21.));
#12197=CARTESIAN_POINT('Ctrl Pts',(-19.6780827744426,-7.61336212350879,
0.));
#12198=CARTESIAN_POINT('Ctrl Pts',(-19.6780827744426,-7.61336212350879,
21.));
#12199=CARTESIAN_POINT('Ctrl Pts',(-19.6274933688524,-7.6184403707059,0.));
#12200=CARTESIAN_POINT('Ctrl Pts',(-19.6274933688524,-7.6184403707059,21.));
#12201=CARTESIAN_POINT('Ctrl Pts',(-19.5769527121826,-7.62324053735219,
0.));
#12202=CARTESIAN_POINT('Ctrl Pts',(-19.5769527121826,-7.62324053735219,
21.));
#12203=CARTESIAN_POINT('Ctrl Pts',(-19.5264621687521,-7.62776096538882,
0.));
#12204=CARTESIAN_POINT('Ctrl Pts',(-19.5264621687521,-7.62776096538882,
21.));
#12205=CARTESIAN_POINT('Ctrl Pts',(-19.4760231231881,-7.63199992715365,
0.));
#12206=CARTESIAN_POINT('Ctrl Pts',(-19.4760231231881,-7.63199992715365,
21.));
#12207=CARTESIAN_POINT('Ctrl Pts',(-19.4256370121006,-7.63595554930653,
0.));
#12208=CARTESIAN_POINT('Ctrl Pts',(-19.4256370121006,-7.63595554930653,
21.));
#12209=CARTESIAN_POINT('Ctrl Pts',(-19.3753053524647,-7.6396257482276,0.));
#12210=CARTESIAN_POINT('Ctrl Pts',(-19.3753053524647,-7.6396257482276,21.));
#12211=CARTESIAN_POINT('Ctrl Pts',(-19.3250297839295,-7.64300812875338,
0.));
#12212=CARTESIAN_POINT('Ctrl Pts',(-19.3250297839295,-7.64300812875338,
21.));
#12213=CARTESIAN_POINT('Ctrl Pts',(-19.2748120456486,-7.64610005549613,
0.));
#12214=CARTESIAN_POINT('Ctrl Pts',(-19.2748120456486,-7.64610005549613,
21.));
#12215=CARTESIAN_POINT('Ctrl Pts',(-19.224653915265,-7.64889882291923,0.));
#12216=CARTESIAN_POINT('Ctrl Pts',(-19.224653915265,-7.64889882291923,21.));
#12217=CARTESIAN_POINT('Ctrl Pts',(-19.1745571539291,-7.65140181220525,
0.));
#12218=CARTESIAN_POINT('Ctrl Pts',(-19.1745571539291,-7.65140181220525,
21.));
#12219=CARTESIAN_POINT('Ctrl Pts',(-19.1245234597312,-7.65360662280608,
0.));
#12220=CARTESIAN_POINT('Ctrl Pts',(-19.1245234597312,-7.65360662280608,
21.));
#12221=CARTESIAN_POINT('Ctrl Pts',(-19.0745543888799,-7.65551129907201,
0.));
#12222=CARTESIAN_POINT('Ctrl Pts',(-19.0745543888799,-7.65551129907201,
21.));
#12223=CARTESIAN_POINT('Ctrl Pts',(-19.0246514144531,-7.65711415727855,
0.));
#12224=CARTESIAN_POINT('Ctrl Pts',(-19.0246514144531,-7.65711415727855,
21.));
#12225=CARTESIAN_POINT('Ctrl Pts',(-18.974816073814,-7.65841335587266,0.));
#12226=CARTESIAN_POINT('Ctrl Pts',(-18.974816073814,-7.65841335587266,21.));
#12227=CARTESIAN_POINT('Ctrl Pts',(-18.9250501008887,-7.65940650980098,
0.));
#12228=CARTESIAN_POINT('Ctrl Pts',(-18.9250501008887,-7.65940650980098,
21.));
#12229=CARTESIAN_POINT('Ctrl Pts',(-18.8753555389435,-7.66009036321663,
0.));
#12230=CARTESIAN_POINT('Ctrl Pts',(-18.8753555389435,-7.66009036321663,
21.));
#12231=CARTESIAN_POINT('Ctrl Pts',(-18.8257349246207,-7.66046025294774,
0.));
#12232=CARTESIAN_POINT('Ctrl Pts',(-18.8257349246207,-7.66046025294774,
21.));
#12233=CARTESIAN_POINT('Ctrl Pts',(-18.7761911671591,-7.6605104692254,0.));
#12234=CARTESIAN_POINT('Ctrl Pts',(-18.7761911671591,-7.6605104692254,21.));
#12235=CARTESIAN_POINT('Ctrl Pts',(-18.7267272235231,-7.66023521705904,
0.));
#12236=CARTESIAN_POINT('Ctrl Pts',(-18.7267272235231,-7.66023521705904,
21.));
#12237=CARTESIAN_POINT('Ctrl Pts',(-18.6773458057584,-7.65962948375621,
0.));
#12238=CARTESIAN_POINT('Ctrl Pts',(-18.6773458057584,-7.65962948375621,
21.));
#12239=CARTESIAN_POINT('Ctrl Pts',(-18.6280491346907,-7.65868976978871,
0.));
#12240=CARTESIAN_POINT('Ctrl Pts',(-18.6280491346907,-7.65868976978871,
21.));
#12241=CARTESIAN_POINT('Ctrl Pts',(-18.5788385228928,-7.65741532450727,
0.));
#12242=CARTESIAN_POINT('Ctrl Pts',(-18.5788385228928,-7.65741532450727,
21.));
#12243=CARTESIAN_POINT('Ctrl Pts',(-18.5297146894905,-7.65580722110436,
0.));
#12244=CARTESIAN_POINT('Ctrl Pts',(-18.5297146894905,-7.65580722110436,
21.));
#12245=CARTESIAN_POINT('Ctrl Pts',(-18.4806785483052,-7.65386603444742,
0.));
#12246=CARTESIAN_POINT('Ctrl Pts',(-18.4806785483052,-7.65386603444742,
21.));
#12247=CARTESIAN_POINT('Ctrl Pts',(-18.4317319183719,-7.65158974829126,
0.));
#12248=CARTESIAN_POINT('Ctrl Pts',(-18.4317319183719,-7.65158974829126,
21.));
#12249=CARTESIAN_POINT('Ctrl Pts',(-18.3828781275628,-7.6489719793775,0.));
#12250=CARTESIAN_POINT('Ctrl Pts',(-18.3828781275628,-7.6489719793775,21.));
#12251=CARTESIAN_POINT('Ctrl Pts',(-18.3341230095852,-7.64599903846601,
0.));
#12252=CARTESIAN_POINT('Ctrl Pts',(-18.3341230095852,-7.64599903846601,
21.));
#12253=CARTESIAN_POINT('Ctrl Pts',(-18.2854741391282,-7.64265220270759,
0.));
#12254=CARTESIAN_POINT('Ctrl Pts',(-18.2854741391282,-7.64265220270759,
21.));
#12255=CARTESIAN_POINT('Ctrl Pts',(-18.2369390502576,-7.63891299603826,
0.));
#12256=CARTESIAN_POINT('Ctrl Pts',(-18.2369390502576,-7.63891299603826,
21.));
#12257=CARTESIAN_POINT('Ctrl Pts',(-18.1885236169197,-7.63476798969016,
0.));
#12258=CARTESIAN_POINT('Ctrl Pts',(-18.1885236169197,-7.63476798969016,
21.));
#12259=CARTESIAN_POINT('Ctrl Pts',(-18.1402306858819,-7.63021285851761,
0.));
#12260=CARTESIAN_POINT('Ctrl Pts',(-18.1402306858819,-7.63021285851761,
21.));
#12261=CARTESIAN_POINT('Ctrl Pts',(-18.0920577897363,-7.62525915358073,
0.));
#12262=CARTESIAN_POINT('Ctrl Pts',(-18.0920577897363,-7.62525915358073,
21.));
#12263=CARTESIAN_POINT('Ctrl Pts',(-18.0439992897906,-7.61992799636654,
0.));
#12264=CARTESIAN_POINT('Ctrl Pts',(-18.0439992897906,-7.61992799636654,
21.));
#12265=CARTESIAN_POINT('Ctrl Pts',(-17.9960506269561,-7.61423755067037,
0.));
#12266=CARTESIAN_POINT('Ctrl Pts',(-17.9960506269561,-7.61423755067037,
21.));
#12267=CARTESIAN_POINT('Ctrl Pts',(-17.9482122228183,-7.60819152580111,
0.));
#12268=CARTESIAN_POINT('Ctrl Pts',(-17.9482122228183,-7.60819152580111,
21.));
#12269=CARTESIAN_POINT('Ctrl Pts',(-17.900492838997,-7.60176928403058,0.));
#12270=CARTESIAN_POINT('Ctrl Pts',(-17.900492838997,-7.60176928403058,21.));
#12271=CARTESIAN_POINT('Ctrl Pts',(-17.8529149331931,-7.59491004201955,
0.));
#12272=CARTESIAN_POINT('Ctrl Pts',(-17.8529149331931,-7.59491004201955,
21.));
#12273=CARTESIAN_POINT('Ctrl Pts',(-17.8055090348024,-7.58752955799498,
0.));
#12274=CARTESIAN_POINT('Ctrl Pts',(-17.8055090348024,-7.58752955799498,
21.));
#12275=CARTESIAN_POINT('Ctrl Pts',(-17.7583042294209,-7.57954834582803,
0.));
#12276=CARTESIAN_POINT('Ctrl Pts',(-17.7583042294209,-7.57954834582803,
21.));
#12277=CARTESIAN_POINT('Ctrl Pts',(-17.7113192869136,-7.57091795530423,
0.));
#12278=CARTESIAN_POINT('Ctrl Pts',(-17.7113192869136,-7.57091795530423,
21.));
#12279=CARTESIAN_POINT('Ctrl Pts',(-17.6645549117314,-7.56164400295862,
0.));
#12280=CARTESIAN_POINT('Ctrl Pts',(-17.6645549117314,-7.56164400295862,
21.));
#12281=CARTESIAN_POINT('Ctrl Pts',(-17.6179818599248,-7.55182125346563,
0.));
#12282=CARTESIAN_POINT('Ctrl Pts',(-17.6179818599248,-7.55182125346563,
21.));
#12283=CARTESIAN_POINT('Ctrl Pts',(-17.5715579419204,-7.54158441095317,
0.));
#12284=CARTESIAN_POINT('Ctrl Pts',(-17.5715579419204,-7.54158441095317,
21.));
#12285=CARTESIAN_POINT('Ctrl Pts',(-17.5252518287336,-7.53103903007863,
0.));
#12286=CARTESIAN_POINT('Ctrl Pts',(-17.5252518287336,-7.53103903007863,
21.));
#12287=CARTESIAN_POINT('Ctrl Pts',(-17.4790653226646,-7.52019696747328,
0.));
#12288=CARTESIAN_POINT('Ctrl Pts',(-17.4790653226646,-7.52019696747328,
21.));
#12289=CARTESIAN_POINT('Ctrl Pts',(-17.4330545448126,-7.50891486634214,
0.));
#12290=CARTESIAN_POINT('Ctrl Pts',(-17.4330545448126,-7.50891486634214,
21.));
#12291=CARTESIAN_POINT('Ctrl Pts',(-17.3873563447297,-7.4968177445175,0.));
#12292=CARTESIAN_POINT('Ctrl Pts',(-17.3873563447297,-7.4968177445175,21.));
#12293=CARTESIAN_POINT('Ctrl Pts',(-17.3421522689127,-7.48340100912745,
0.));
#12294=CARTESIAN_POINT('Ctrl Pts',(-17.3421522689127,-7.48340100912745,
21.));
#12295=CARTESIAN_POINT('Ctrl Pts',(-17.3065305096784,-7.47120323460919,
0.));
#12296=CARTESIAN_POINT('Ctrl Pts',(-17.3065305096784,-7.47120323460919,
21.));
#12297=CARTESIAN_POINT('Ctrl Pts',(-17.2801832097582,-7.4610504981825,0.));
#12298=CARTESIAN_POINT('Ctrl Pts',(-17.2801832097582,-7.4610504981825,21.));
#12299=CARTESIAN_POINT('Ctrl Pts',(-17.2627905583523,-7.45381253347183,
0.));
#12300=CARTESIAN_POINT('Ctrl Pts',(-17.2627905583523,-7.45381253347183,
21.));
#12301=CARTESIAN_POINT('Ctrl Pts',(-17.2541372868972,-7.45007618140238,
0.));
#12302=CARTESIAN_POINT('Ctrl Pts',(-17.2541372868972,-7.45007618140238,
21.));
#12303=CARTESIAN_POINT('',(-20.698113262342,-7.45574324794406,0.));
#12304=CARTESIAN_POINT('Ctrl Pts',(-17.2541372868972,-7.45007618140238,
0.));
#12305=CARTESIAN_POINT('Ctrl Pts',(-17.2627905583523,-7.45381253347183,
0.));
#12306=CARTESIAN_POINT('Ctrl Pts',(-17.2801832097582,-7.4610504981825,0.));
#12307=CARTESIAN_POINT('Ctrl Pts',(-17.3065305096784,-7.47120323460919,
0.));
#12308=CARTESIAN_POINT('Ctrl Pts',(-17.3421522689127,-7.48340100912745,
0.));
#12309=CARTESIAN_POINT('Ctrl Pts',(-17.3873563447297,-7.4968177445175,0.));
#12310=CARTESIAN_POINT('Ctrl Pts',(-17.4330545448126,-7.50891486634214,
0.));
#12311=CARTESIAN_POINT('Ctrl Pts',(-17.4790653226646,-7.52019696747328,
0.));
#12312=CARTESIAN_POINT('Ctrl Pts',(-17.5252518287336,-7.53103903007863,
0.));
#12313=CARTESIAN_POINT('Ctrl Pts',(-17.5715579419204,-7.54158441095317,
0.));
#12314=CARTESIAN_POINT('Ctrl Pts',(-17.6179818599248,-7.55182125346563,
0.));
#12315=CARTESIAN_POINT('Ctrl Pts',(-17.6645549117314,-7.56164400295862,
0.));
#12316=CARTESIAN_POINT('Ctrl Pts',(-17.7113192869136,-7.57091795530423,
0.));
#12317=CARTESIAN_POINT('Ctrl Pts',(-17.7583042294209,-7.57954834582803,
0.));
#12318=CARTESIAN_POINT('Ctrl Pts',(-17.8055090348024,-7.58752955799498,
0.));
#12319=CARTESIAN_POINT('Ctrl Pts',(-17.8529149331931,-7.59491004201955,
0.));
#12320=CARTESIAN_POINT('Ctrl Pts',(-17.900492838997,-7.60176928403058,0.));
#12321=CARTESIAN_POINT('Ctrl Pts',(-17.9482122228183,-7.60819152580111,
0.));
#12322=CARTESIAN_POINT('Ctrl Pts',(-17.9960506269561,-7.61423755067037,
0.));
#12323=CARTESIAN_POINT('Ctrl Pts',(-18.0439992897906,-7.61992799636654,
0.));
#12324=CARTESIAN_POINT('Ctrl Pts',(-18.0920577897363,-7.62525915358073,
0.));
#12325=CARTESIAN_POINT('Ctrl Pts',(-18.1402306858819,-7.63021285851761,
0.));
#12326=CARTESIAN_POINT('Ctrl Pts',(-18.1885236169197,-7.63476798969016,
0.));
#12327=CARTESIAN_POINT('Ctrl Pts',(-18.2369390502576,-7.63891299603826,
0.));
#12328=CARTESIAN_POINT('Ctrl Pts',(-18.2854741391282,-7.64265220270759,
0.));
#12329=CARTESIAN_POINT('Ctrl Pts',(-18.3341230095852,-7.64599903846601,
0.));
#12330=CARTESIAN_POINT('Ctrl Pts',(-18.3828781275628,-7.6489719793775,0.));
#12331=CARTESIAN_POINT('Ctrl Pts',(-18.4317319183719,-7.65158974829126,
0.));
#12332=CARTESIAN_POINT('Ctrl Pts',(-18.4806785483052,-7.65386603444742,
0.));
#12333=CARTESIAN_POINT('Ctrl Pts',(-18.5297146894905,-7.65580722110436,
0.));
#12334=CARTESIAN_POINT('Ctrl Pts',(-18.5788385228928,-7.65741532450727,
0.));
#12335=CARTESIAN_POINT('Ctrl Pts',(-18.6280491346907,-7.65868976978871,
0.));
#12336=CARTESIAN_POINT('Ctrl Pts',(-18.6773458057584,-7.65962948375621,
0.));
#12337=CARTESIAN_POINT('Ctrl Pts',(-18.7267272235231,-7.66023521705904,
0.));
#12338=CARTESIAN_POINT('Ctrl Pts',(-18.7761911671591,-7.6605104692254,0.));
#12339=CARTESIAN_POINT('Ctrl Pts',(-18.8257349246207,-7.66046025294774,
0.));
#12340=CARTESIAN_POINT('Ctrl Pts',(-18.8753555389435,-7.66009036321663,
0.));
#12341=CARTESIAN_POINT('Ctrl Pts',(-18.9250501008887,-7.65940650980098,
0.));
#12342=CARTESIAN_POINT('Ctrl Pts',(-18.974816073814,-7.65841335587266,0.));
#12343=CARTESIAN_POINT('Ctrl Pts',(-19.0246514144531,-7.65711415727855,
0.));
#12344=CARTESIAN_POINT('Ctrl Pts',(-19.0745543888799,-7.65551129907201,
0.));
#12345=CARTESIAN_POINT('Ctrl Pts',(-19.1245234597312,-7.65360662280608,
0.));
#12346=CARTESIAN_POINT('Ctrl Pts',(-19.1745571539291,-7.65140181220525,
0.));
#12347=CARTESIAN_POINT('Ctrl Pts',(-19.224653915265,-7.64889882291923,0.));
#12348=CARTESIAN_POINT('Ctrl Pts',(-19.2748120456486,-7.64610005549613,
0.));
#12349=CARTESIAN_POINT('Ctrl Pts',(-19.3250297839295,-7.64300812875338,
0.));
#12350=CARTESIAN_POINT('Ctrl Pts',(-19.3753053524647,-7.6396257482276,0.));
#12351=CARTESIAN_POINT('Ctrl Pts',(-19.4256370121006,-7.63595554930653,
0.));
#12352=CARTESIAN_POINT('Ctrl Pts',(-19.4760231231881,-7.63199992715365,
0.));
#12353=CARTESIAN_POINT('Ctrl Pts',(-19.5264621687521,-7.62776096538882,
0.));
#12354=CARTESIAN_POINT('Ctrl Pts',(-19.5769527121826,-7.62324053735219,
0.));
#12355=CARTESIAN_POINT('Ctrl Pts',(-19.6274933688524,-7.6184403707059,0.));
#12356=CARTESIAN_POINT('Ctrl Pts',(-19.6780827744426,-7.61336212350879,
0.));
#12357=CARTESIAN_POINT('Ctrl Pts',(-19.7287195480601,-7.60800746969261,
0.));
#12358=CARTESIAN_POINT('Ctrl Pts',(-19.7794022782484,-7.60237814110186,
0.));
#12359=CARTESIAN_POINT('Ctrl Pts',(-19.830129556152,-7.59647587605448,0.));
#12360=CARTESIAN_POINT('Ctrl Pts',(-19.8808999994024,-7.59030238888852,
0.));
#12361=CARTESIAN_POINT('Ctrl Pts',(-19.931712276832,-7.58385933533351,0.));
#12362=CARTESIAN_POINT('Ctrl Pts',(-19.9825651387294,-7.57714827622806,
0.));
#12363=CARTESIAN_POINT('Ctrl Pts',(-20.0334574248557,-7.57017066105972,
0.));
#12364=CARTESIAN_POINT('Ctrl Pts',(-20.0843880130978,-7.5629278654946,0.));
#12365=CARTESIAN_POINT('Ctrl Pts',(-20.1353557774357,-7.55542122125494,
0.));
#12366=CARTESIAN_POINT('Ctrl Pts',(-20.1863595454674,-7.54765204869254,
0.));
#12367=CARTESIAN_POINT('Ctrl Pts',(-20.2373980474879,-7.53962169534166,
0.));
#12368=CARTESIAN_POINT('Ctrl Pts',(-20.2884698940944,-7.53133155804007,
0.));
#12369=CARTESIAN_POINT('Ctrl Pts',(-20.3395736743243,-7.52278303006887,
0.));
#12370=CARTESIAN_POINT('Ctrl Pts',(-20.3907080367098,-7.51397746081993,
0.));
#12371=CARTESIAN_POINT('Ctrl Pts',(-20.4418717748497,-7.50491611266253,
0.));
#12372=CARTESIAN_POINT('Ctrl Pts',(-20.4930639156161,-7.49560012018405,
0.));
#12373=CARTESIAN_POINT('Ctrl Pts',(-20.5545277683621,-7.48411651832412,
0.));
#12374=CARTESIAN_POINT('Ctrl Pts',(-20.6057817877246,-7.47423073598681,
0.));
#12375=CARTESIAN_POINT('Ctrl Pts',(-20.6468066077586,-7.46612041736313,
0.));
#12376=CARTESIAN_POINT('Ctrl Pts',(-20.6775873630604,-7.45992433946823,
0.));
#12377=CARTESIAN_POINT('Ctrl Pts',(-20.698113262342,-7.455743247944,0.));
#12378=CARTESIAN_POINT('',(-20.698113262342,-7.45574324794406,13.));
#12379=CARTESIAN_POINT('Ctrl Pts',(-20.698113262342,-7.455743247944,13.));
#12380=CARTESIAN_POINT('Ctrl Pts',(-20.5970733933809,-7.47632490106067,
13.));
#12381=CARTESIAN_POINT('Ctrl Pts',(-20.496187784905,-7.49544541955086,13.));
#12382=CARTESIAN_POINT('Ctrl Pts',(-20.3954689842507,-7.51308219823823,
13.));
#12383=CARTESIAN_POINT('Ctrl Pts',(-20.2285735577406,-7.54230710641993,
13.));
#12384=CARTESIAN_POINT('Ctrl Pts',(-20.0621477325708,-7.5674509566436,13.));
#12385=CARTESIAN_POINT('Ctrl Pts',(-19.8963869140364,-7.58830059883611,
13.));
#12386=CARTESIAN_POINT('Ctrl Pts',(-19.7689734275332,-7.60432685659461,
13.));
#12387=CARTESIAN_POINT('Ctrl Pts',(-19.6419503956054,-7.61781485408936,
13.));
#12388=CARTESIAN_POINT('Ctrl Pts',(-19.5154161657059,-7.6286436791923,13.));
#12389=CARTESIAN_POINT('Ctrl Pts',(-19.3792051127088,-7.64030064878198,
13.));
#12390=CARTESIAN_POINT('Ctrl Pts',(-19.2435576448926,-7.64888186434619,
13.));
#12391=CARTESIAN_POINT('Ctrl Pts',(-19.1086228836126,-7.65417053742023,
13.));
#12392=CARTESIAN_POINT('Ctrl Pts',(-19.0339193365638,-7.65709849041074,
13.));
#12393=CARTESIAN_POINT('Ctrl Pts',(-18.9594327323946,-7.65902218171137,
13.));
#12394=CARTESIAN_POINT('Ctrl Pts',(-18.8851905417994,-7.65990167998082,
13.));
#12395=CARTESIAN_POINT('Ctrl Pts',(-18.813647852512,-7.6607491990386,13.));
#12396=CARTESIAN_POINT('Ctrl Pts',(-18.7423342827731,-7.66062065572261,
13.));
#12397=CARTESIAN_POINT('Ctrl Pts',(-18.6712863088345,-7.65944821269773,
13.));
#12398=CARTESIAN_POINT('Ctrl Pts',(-18.6098790720615,-7.65843486238751,
13.));
#12399=CARTESIAN_POINT('Ctrl Pts',(-18.5486691990401,-7.65664478981881,
13.));
#12400=CARTESIAN_POINT('Ctrl Pts',(-18.487665984844,-7.65407864069299,13.));
#12401=CARTESIAN_POINT('Ctrl Pts',(-18.4438867380777,-7.65223703156962,
13.));
#12402=CARTESIAN_POINT('Ctrl Pts',(-18.4002130326034,-7.64999840196622,
13.));
#12403=CARTESIAN_POINT('Ctrl Pts',(-18.3566609382467,-7.64732656561704,
13.));
#12404=CARTESIAN_POINT('Ctrl Pts',(-18.3138180356583,-7.6446982368046,13.));
#12405=CARTESIAN_POINT('Ctrl Pts',(-18.2710948572002,-7.64164464439117,
13.));
#12406=CARTESIAN_POINT('Ctrl Pts',(-18.2285117407113,-7.63811742043515,
13.));
#12407=CARTESIAN_POINT('Ctrl Pts',(-18.1915896769364,-7.63505911003915,
13.));
#12408=CARTESIAN_POINT('Ctrl Pts',(-18.1547737063835,-7.63164238135661,
13.));
#12409=CARTESIAN_POINT('Ctrl Pts',(-18.1180614603993,-7.62788266165657,
13.));
#12410=CARTESIAN_POINT('Ctrl Pts',(-18.0848085885333,-7.62447721821159,
13.));
#12411=CARTESIAN_POINT('Ctrl Pts',(-18.0516390295742,-7.62079564899676,
13.));
#12412=CARTESIAN_POINT('Ctrl Pts',(-18.0185473583857,-7.61686093606607,
13.));
#12413=CARTESIAN_POINT('Ctrl Pts',(-17.9906726825976,-7.61354654173896,
13.));
#12414=CARTESIAN_POINT('Ctrl Pts',(-17.9628527173259,-7.61005417561197,
13.));
#12415=CARTESIAN_POINT('Ctrl Pts',(-17.935095231232,-7.60636550499839,13.));
#12416=CARTESIAN_POINT('Ctrl Pts',(-17.8949271288068,-7.60102759728881,
13.));
#12417=CARTESIAN_POINT('Ctrl Pts',(-17.8548900767542,-7.5952778259702,13.));
#12418=CARTESIAN_POINT('Ctrl Pts',(-17.8150590780368,-7.58891067826985,
13.));
#12419=CARTESIAN_POINT('Ctrl Pts',(-17.7909916433023,-7.58506340060529,
13.));
#12420=CARTESIAN_POINT('Ctrl Pts',(-17.7670005718664,-7.58098742040678,
13.));
#12421=CARTESIAN_POINT('Ctrl Pts',(-17.743095591428,-7.57665817622453,13.));
#12422=CARTESIAN_POINT('Ctrl Pts',(-17.7210484745798,-7.57266539519733,
13.));
#12423=CARTESIAN_POINT('Ctrl Pts',(-17.6990750119521,-7.5684559326956,13.));
#12424=CARTESIAN_POINT('Ctrl Pts',(-17.6771683095201,-7.56405390355785,
13.));
#12425=CARTESIAN_POINT('Ctrl Pts',(-17.6470334201915,-7.55799846635553,
13.));
#12426=CARTESIAN_POINT('Ctrl Pts',(-17.6170224066021,-7.55158552707305,
13.));
#12427=CARTESIAN_POINT('Ctrl Pts',(-17.5870909089238,-7.54495919885366,
13.));
#12428=CARTESIAN_POINT('Ctrl Pts',(-17.5681018329048,-7.54075533803665,
13.));
#12429=CARTESIAN_POINT('Ctrl Pts',(-17.5491442490796,-7.53646718585433,
13.));
#12430=CARTESIAN_POINT('Ctrl Pts',(-17.5302169633081,-7.53210330802969,
13.));
#12431=CARTESIAN_POINT('Ctrl Pts',(-17.5132306053115,-7.52818693080173,
13.));
#12432=CARTESIAN_POINT('Ctrl Pts',(-17.4962684160869,-7.52421025221118,
13.));
#12433=CARTESIAN_POINT('Ctrl Pts',(-17.4793429835075,-7.52014106530203,
13.));
#12434=CARTESIAN_POINT('Ctrl Pts',(-17.4615509829577,-7.51586353943172,
13.));
#12435=CARTESIAN_POINT('Ctrl Pts',(-17.4437995539221,-7.51148394209351,
13.));
#12436=CARTESIAN_POINT('Ctrl Pts',(-17.4261238143002,-7.50690601560406,
13.));
#12437=CARTESIAN_POINT('Ctrl Pts',(-17.3967644499127,-7.49930208983814,
13.));
#12438=CARTESIAN_POINT('Ctrl Pts',(-17.367616818873,-7.49114308213498,13.));
#12439=CARTESIAN_POINT('Ctrl Pts',(-17.3388922514848,-7.48183975621699,
13.));
#12440=CARTESIAN_POINT('Ctrl Pts',(-17.3230525027431,-7.47670957120807,
13.));
#12441=CARTESIAN_POINT('Ctrl Pts',(-17.3073418194459,-7.47123011544593,
13.));
#12442=CARTESIAN_POINT('Ctrl Pts',(-17.2917860605524,-7.46532888197223,
13.));
#12443=CARTESIAN_POINT('Ctrl Pts',(-17.2791322530001,-7.46052853290484,
13.));
#12444=CARTESIAN_POINT('Ctrl Pts',(-17.2665809316714,-7.45544915948875,
13.));
#12445=CARTESIAN_POINT('Ctrl Pts',(-17.2541372868972,-7.45007618140238,
13.));
#12446=CARTESIAN_POINT('',(-20.698113262342,-7.45574324794406,0.));
#12447=CARTESIAN_POINT('Origin',(-5.38923623413286E-12,-1.75106900012182E-12,
0.));
#12448=CARTESIAN_POINT('',(-21.1275013067528,-6.1342227326009,0.));
#12449=CARTESIAN_POINT('Origin',(-5.38923623413286E-12,-1.75106900012182E-12,
0.));
#12450=CARTESIAN_POINT('',(-21.1275013067528,-6.1342227326009,13.));
#12451=CARTESIAN_POINT('Origin',(-5.38923623413286E-12,-1.75106900012182E-12,
13.));
#12452=CARTESIAN_POINT('',(-21.1275013067528,-6.1342227326009,0.));
#12453=CARTESIAN_POINT('Ctrl Pts',(-18.337935196262,-4.1144891981253,0.));
#12454=CARTESIAN_POINT('Ctrl Pts',(-18.337935196262,-4.1144891981253,21.));
#12455=CARTESIAN_POINT('Ctrl Pts',(-18.3471320125699,-4.11655269114951,
0.));
#12456=CARTESIAN_POINT('Ctrl Pts',(-18.3471320125699,-4.11655269114951,
21.));
#12457=CARTESIAN_POINT('Ctrl Pts',(-18.3654573320481,-4.12092019868859,
0.));
#12458=CARTESIAN_POINT('Ctrl Pts',(-18.3654573320481,-4.12092019868859,
21.));
#12459=CARTESIAN_POINT('Ctrl Pts',(-18.3927403741815,-4.12819301671078,
0.));
#12460=CARTESIAN_POINT('Ctrl Pts',(-18.3927403741815,-4.12819301671078,
21.));
#12461=CARTESIAN_POINT('Ctrl Pts',(-18.4287286547442,-4.13926275457062,
0.));
#12462=CARTESIAN_POINT('Ctrl Pts',(-18.4287286547442,-4.13926275457062,
21.));
#12463=CARTESIAN_POINT('Ctrl Pts',(-18.4731856794913,-4.15497867673974,
0.));
#12464=CARTESIAN_POINT('Ctrl Pts',(-18.4731856794913,-4.15497867673974,
21.));
#12465=CARTESIAN_POINT('Ctrl Pts',(-18.5172668097744,-4.17205262766561,
0.));
#12466=CARTESIAN_POINT('Ctrl Pts',(-18.5172668097744,-4.17205262766561,
21.));
#12467=CARTESIAN_POINT('Ctrl Pts',(-18.5611217636409,-4.1899696727862,0.));
#12468=CARTESIAN_POINT('Ctrl Pts',(-18.5611217636409,-4.1899696727862,21.));
#12469=CARTESIAN_POINT('Ctrl Pts',(-18.6048602364653,-4.20834600700664,
0.));
#12470=CARTESIAN_POINT('Ctrl Pts',(-18.6048602364653,-4.20834600700664,
21.));
#12471=CARTESIAN_POINT('Ctrl Pts',(-18.6485210883348,-4.22703266508918,
0.));
#12472=CARTESIAN_POINT('Ctrl Pts',(-18.6485210883348,-4.22703266508918,
21.));
#12473=CARTESIAN_POINT('Ctrl Pts',(-18.6920958920047,-4.24603817988452,
0.));
#12474=CARTESIAN_POINT('Ctrl Pts',(-18.6920958920047,-4.24603817988452,
21.));
#12475=CARTESIAN_POINT('Ctrl Pts',(-18.735547949685,-4.26546636161932,0.));
#12476=CARTESIAN_POINT('Ctrl Pts',(-18.735547949685,-4.26546636161932,21.));
#12477=CARTESIAN_POINT('Ctrl Pts',(-18.778832216358,-4.28545098663153,0.));
#12478=CARTESIAN_POINT('Ctrl Pts',(-18.778832216358,-4.28545098663153,21.));
#12479=CARTESIAN_POINT('Ctrl Pts',(-18.8219166495975,-4.30608591031525,
0.));
#12480=CARTESIAN_POINT('Ctrl Pts',(-18.8219166495975,-4.30608591031525,
21.));
#12481=CARTESIAN_POINT('Ctrl Pts',(-18.8647973781745,-4.32737526247704,
0.));
#12482=CARTESIAN_POINT('Ctrl Pts',(-18.8647973781745,-4.32737526247704,
21.));
#12483=CARTESIAN_POINT('Ctrl Pts',(-18.9074876952706,-4.34926881342021,
0.));
#12484=CARTESIAN_POINT('Ctrl Pts',(-18.9074876952706,-4.34926881342021,
21.));
#12485=CARTESIAN_POINT('Ctrl Pts',(-18.9500107909187,-4.37168516143122,
0.));
#12486=CARTESIAN_POINT('Ctrl Pts',(-18.9500107909187,-4.37168516143122,
21.));
#12487=CARTESIAN_POINT('Ctrl Pts',(-18.9923914823906,-4.39453820875554,
0.));
#12488=CARTESIAN_POINT('Ctrl Pts',(-18.9923914823906,-4.39453820875554,
21.));
#12489=CARTESIAN_POINT('Ctrl Pts',(-19.034647328575,-4.41776558033331,0.));
#12490=CARTESIAN_POINT('Ctrl Pts',(-19.034647328575,-4.41776558033331,21.));
#12491=CARTESIAN_POINT('Ctrl Pts',(-19.0767833717249,-4.44134542994081,
0.));
#12492=CARTESIAN_POINT('Ctrl Pts',(-19.0767833717249,-4.44134542994081,
21.));
#12493=CARTESIAN_POINT('Ctrl Pts',(-19.1187970904933,-4.46528051067021,
0.));
#12494=CARTESIAN_POINT('Ctrl Pts',(-19.1187970904933,-4.46528051067021,
21.));
#12495=CARTESIAN_POINT('Ctrl Pts',(-19.1606814968494,-4.48958819710576,
0.));
#12496=CARTESIAN_POINT('Ctrl Pts',(-19.1606814968494,-4.48958819710576,
21.));
#12497=CARTESIAN_POINT('Ctrl Pts',(-19.2024287376926,-4.51428889122954,
0.));
#12498=CARTESIAN_POINT('Ctrl Pts',(-19.2024287376926,-4.51428889122954,
21.));
#12499=CARTESIAN_POINT('Ctrl Pts',(-19.2440340196551,-4.53939338835151,
0.));
#12500=CARTESIAN_POINT('Ctrl Pts',(-19.2440340196551,-4.53939338835151,
21.));
#12501=CARTESIAN_POINT('Ctrl Pts',(-19.2854975819105,-4.5648965160674,0.));
#12502=CARTESIAN_POINT('Ctrl Pts',(-19.2854975819105,-4.5648965160674,21.));
#12503=CARTESIAN_POINT('Ctrl Pts',(-19.3268225655679,-4.59078395765677,
0.));
#12504=CARTESIAN_POINT('Ctrl Pts',(-19.3268225655679,-4.59078395765677,
21.));
#12505=CARTESIAN_POINT('Ctrl Pts',(-19.3680137353983,-4.61703633725711,
0.));
#12506=CARTESIAN_POINT('Ctrl Pts',(-19.3680137353983,-4.61703633725711,
21.));
#12507=CARTESIAN_POINT('Ctrl Pts',(-19.4090759683639,-4.64363405547472,
0.));
#12508=CARTESIAN_POINT('Ctrl Pts',(-19.4090759683639,-4.64363405547472,
21.));
#12509=CARTESIAN_POINT('Ctrl Pts',(-19.4500125912299,-4.67056260851453,
0.));
#12510=CARTESIAN_POINT('Ctrl Pts',(-19.4500125912299,-4.67056260851453,
21.));
#12511=CARTESIAN_POINT('Ctrl Pts',(-19.4908246636763,-4.69781487613784,
0.));
#12512=CARTESIAN_POINT('Ctrl Pts',(-19.4908246636763,-4.69781487613784,
21.));
#12513=CARTESIAN_POINT('Ctrl Pts',(-19.531511899192,-4.72538815796615,0.));
#12514=CARTESIAN_POINT('Ctrl Pts',(-19.531511899192,-4.72538815796615,21.));
#12515=CARTESIAN_POINT('Ctrl Pts',(-19.5720732205813,-4.7532823819461,0.));
#12516=CARTESIAN_POINT('Ctrl Pts',(-19.5720732205813,-4.7532823819461,21.));
#12517=CARTESIAN_POINT('Ctrl Pts',(-19.6125074152527,-4.7814979936173,0.));
#12518=CARTESIAN_POINT('Ctrl Pts',(-19.6125074152527,-4.7814979936173,21.));
#12519=CARTESIAN_POINT('Ctrl Pts',(-19.6528138625329,-4.8100336141806,0.));
#12520=CARTESIAN_POINT('Ctrl Pts',(-19.6528138625329,-4.8100336141806,21.));
#12521=CARTESIAN_POINT('Ctrl Pts',(-19.6929928227072,-4.83888510708974,
0.));
#12522=CARTESIAN_POINT('Ctrl Pts',(-19.6929928227072,-4.83888510708974,
21.));
#12523=CARTESIAN_POINT('Ctrl Pts',(-19.7330450480715,-4.86804682289086,
0.));
#12524=CARTESIAN_POINT('Ctrl Pts',(-19.7330450480715,-4.86804682289086,
21.));
#12525=CARTESIAN_POINT('Ctrl Pts',(-19.772971552601,-4.89751233527804,0.));
#12526=CARTESIAN_POINT('Ctrl Pts',(-19.772971552601,-4.89751233527804,21.));
#12527=CARTESIAN_POINT('Ctrl Pts',(-19.8127733387903,-4.92727531494346,
0.));
#12528=CARTESIAN_POINT('Ctrl Pts',(-19.8127733387903,-4.92727531494346,
21.));
#12529=CARTESIAN_POINT('Ctrl Pts',(-19.8524510953961,-4.95733049830095,
0.));
#12530=CARTESIAN_POINT('Ctrl Pts',(-19.8524510953961,-4.95733049830095,
21.));
#12531=CARTESIAN_POINT('Ctrl Pts',(-19.8920050831202,-4.98767405031333,
0.));
#12532=CARTESIAN_POINT('Ctrl Pts',(-19.8920050831202,-4.98767405031333,
21.));
#12533=CARTESIAN_POINT('Ctrl Pts',(-19.931435301086,-5.01830302225557,0.));
#12534=CARTESIAN_POINT('Ctrl Pts',(-19.931435301086,-5.01830302225557,21.));
#12535=CARTESIAN_POINT('Ctrl Pts',(-19.9707415879783,-5.04921502064063,
0.));
#12536=CARTESIAN_POINT('Ctrl Pts',(-19.9707415879783,-5.04921502064063,
21.));
#12537=CARTESIAN_POINT('Ctrl Pts',(-20.0099237417205,-5.08040781745336,
0.));
#12538=CARTESIAN_POINT('Ctrl Pts',(-20.0099237417205,-5.08040781745336,
21.));
#12539=CARTESIAN_POINT('Ctrl Pts',(-20.0489816528155,-5.11187891582334,
0.));
#12540=CARTESIAN_POINT('Ctrl Pts',(-20.0489816528155,-5.11187891582334,
21.));
#12541=CARTESIAN_POINT('Ctrl Pts',(-20.087915358486,-5.14362537555397,0.));
#12542=CARTESIAN_POINT('Ctrl Pts',(-20.087915358486,-5.14362537555397,21.));
#12543=CARTESIAN_POINT('Ctrl Pts',(-20.1267249732337,-5.17564404279921,
0.));
#12544=CARTESIAN_POINT('Ctrl Pts',(-20.1267249732337,-5.17564404279921,
21.));
#12545=CARTESIAN_POINT('Ctrl Pts',(-20.1654106491899,-5.20793168386163,
0.));
#12546=CARTESIAN_POINT('Ctrl Pts',(-20.1654106491899,-5.20793168386163,
21.));
#12547=CARTESIAN_POINT('Ctrl Pts',(-20.2039725283917,-5.2404851444189,0.));
#12548=CARTESIAN_POINT('Ctrl Pts',(-20.2039725283917,-5.2404851444189,21.));
#12549=CARTESIAN_POINT('Ctrl Pts',(-20.2424106921768,-5.2733015229815,0.));
#12550=CARTESIAN_POINT('Ctrl Pts',(-20.2424106921768,-5.2733015229815,21.));
#12551=CARTESIAN_POINT('Ctrl Pts',(-20.2807251380077,-5.30637824220997,
0.));
#12552=CARTESIAN_POINT('Ctrl Pts',(-20.2807251380077,-5.30637824220997,
21.));
#12553=CARTESIAN_POINT('Ctrl Pts',(-20.3189158047642,-5.33971294212213,
0.));
#12554=CARTESIAN_POINT('Ctrl Pts',(-20.3189158047642,-5.33971294212213,
21.));
#12555=CARTESIAN_POINT('Ctrl Pts',(-20.3569825877537,-5.37330341114649,
0.));
#12556=CARTESIAN_POINT('Ctrl Pts',(-20.3569825877537,-5.37330341114649,
21.));
#12557=CARTESIAN_POINT('Ctrl Pts',(-20.3949253578015,-5.40714750595874,
0.));
#12558=CARTESIAN_POINT('Ctrl Pts',(-20.3949253578015,-5.40714750595874,
21.));
#12559=CARTESIAN_POINT('Ctrl Pts',(-20.4327439816542,-5.44124306065111,
0.));
#12560=CARTESIAN_POINT('Ctrl Pts',(-20.4327439816542,-5.44124306065111,
21.));
#12561=CARTESIAN_POINT('Ctrl Pts',(-20.4704383353718,-5.4755878444985,0.));
#12562=CARTESIAN_POINT('Ctrl Pts',(-20.4704383353718,-5.4755878444985,21.));
#12563=CARTESIAN_POINT('Ctrl Pts',(-20.5080083009242,-5.51017962306782,
0.));
#12564=CARTESIAN_POINT('Ctrl Pts',(-20.5080083009242,-5.51017962306782,
21.));
#12565=CARTESIAN_POINT('Ctrl Pts',(-20.5454537676144,-5.5450161968946,0.));
#12566=CARTESIAN_POINT('Ctrl Pts',(-20.5454537676144,-5.5450161968946,21.));
#12567=CARTESIAN_POINT('Ctrl Pts',(-20.5827746317185,-5.58009544402474,
0.));
#12568=CARTESIAN_POINT('Ctrl Pts',(-20.5827746317185,-5.58009544402474,
21.));
#12569=CARTESIAN_POINT('Ctrl Pts',(-20.6199707996366,-5.61541536715149,
0.));
#12570=CARTESIAN_POINT('Ctrl Pts',(-20.6199707996366,-5.61541536715149,
21.));
#12571=CARTESIAN_POINT('Ctrl Pts',(-20.6570421847033,-5.65097411164334,
0.));
#12572=CARTESIAN_POINT('Ctrl Pts',(-20.6570421847033,-5.65097411164334,
21.));
#12573=CARTESIAN_POINT('Ctrl Pts',(-20.6939886877061,-5.68676990500163,
0.));
#12574=CARTESIAN_POINT('Ctrl Pts',(-20.6939886877061,-5.68676990500163,
21.));
#12575=CARTESIAN_POINT('Ctrl Pts',(-20.7308101804425,-5.72280100798241,
0.));
#12576=CARTESIAN_POINT('Ctrl Pts',(-20.7308101804425,-5.72280100798241,
21.));
#12577=CARTESIAN_POINT('Ctrl Pts',(-20.7675064905026,-5.75906566327795,
0.));
#12578=CARTESIAN_POINT('Ctrl Pts',(-20.7675064905026,-5.75906566327795,
21.));
#12579=CARTESIAN_POINT('Ctrl Pts',(-20.8040773827343,-5.79556203439644,
0.));
#12580=CARTESIAN_POINT('Ctrl Pts',(-20.8040773827343,-5.79556203439644,
21.));
#12581=CARTESIAN_POINT('Ctrl Pts',(-20.8405225541277,-5.83228817460177,
0.));
#12582=CARTESIAN_POINT('Ctrl Pts',(-20.8405225541277,-5.83228817460177,
21.));
#12583=CARTESIAN_POINT('Ctrl Pts',(-20.8768416821402,-5.86924212736287,
0.));
#12584=CARTESIAN_POINT('Ctrl Pts',(-20.8768416821402,-5.86924212736287,
21.));
#12585=CARTESIAN_POINT('Ctrl Pts',(-20.9130344665641,-5.90642200662599,
0.));
#12586=CARTESIAN_POINT('Ctrl Pts',(-20.9130344665641,-5.90642200662599,
21.));
#12587=CARTESIAN_POINT('Ctrl Pts',(-20.9491006734021,-5.94382608200804,
0.));
#12588=CARTESIAN_POINT('Ctrl Pts',(-20.9491006734021,-5.94382608200804,
21.));
#12589=CARTESIAN_POINT('Ctrl Pts',(-20.9850401822713,-5.98145286361836,
0.));
#12590=CARTESIAN_POINT('Ctrl Pts',(-20.9850401822713,-5.98145286361836,
21.));
#12591=CARTESIAN_POINT('Ctrl Pts',(-21.0208530236003,-6.01930117633044,
0.));
#12592=CARTESIAN_POINT('Ctrl Pts',(-21.0208530236003,-6.01930117633044,
21.));
#12593=CARTESIAN_POINT('Ctrl Pts',(-21.0565393163693,-6.05737013696532,
0.));
#12594=CARTESIAN_POINT('Ctrl Pts',(-21.0565393163693,-6.05737013696532,
21.));
#12595=CARTESIAN_POINT('Ctrl Pts',(-21.0849872356853,-6.08800133883114,
0.));
#12596=CARTESIAN_POINT('Ctrl Pts',(-21.0849872356853,-6.08800133883114,
21.));
#12597=CARTESIAN_POINT('Ctrl Pts',(-21.1062663590356,-6.11107360216957,
0.));
#12598=CARTESIAN_POINT('Ctrl Pts',(-21.1062663590356,-6.11107360216957,
21.));
#12599=CARTESIAN_POINT('Ctrl Pts',(-21.1204271980506,-6.12649903511517,
0.));
#12600=CARTESIAN_POINT('Ctrl Pts',(-21.1204271980506,-6.12649903511517,
21.));
#12601=CARTESIAN_POINT('Ctrl Pts',(-21.1275013067528,-6.1342227326009,0.));
#12602=CARTESIAN_POINT('Ctrl Pts',(-21.1275013067528,-6.1342227326009,21.));
#12603=CARTESIAN_POINT('Ctrl Pts',(-18.337935196262,-4.1144891981253,0.));
#12604=CARTESIAN_POINT('Ctrl Pts',(-18.3471320125699,-4.11655269114951,
0.));
#12605=CARTESIAN_POINT('Ctrl Pts',(-18.3654573320481,-4.12092019868859,
0.));
#12606=CARTESIAN_POINT('Ctrl Pts',(-18.3927403741815,-4.12819301671078,
0.));
#12607=CARTESIAN_POINT('Ctrl Pts',(-18.4287286547442,-4.13926275457062,
0.));
#12608=CARTESIAN_POINT('Ctrl Pts',(-18.4731856794913,-4.15497867673974,
0.));
#12609=CARTESIAN_POINT('Ctrl Pts',(-18.5172668097744,-4.17205262766561,
0.));
#12610=CARTESIAN_POINT('Ctrl Pts',(-18.5611217636409,-4.1899696727862,0.));
#12611=CARTESIAN_POINT('Ctrl Pts',(-18.6048602364653,-4.20834600700664,
0.));
#12612=CARTESIAN_POINT('Ctrl Pts',(-18.6485210883348,-4.22703266508918,
0.));
#12613=CARTESIAN_POINT('Ctrl Pts',(-18.6920958920047,-4.24603817988452,
0.));
#12614=CARTESIAN_POINT('Ctrl Pts',(-18.735547949685,-4.26546636161932,0.));
#12615=CARTESIAN_POINT('Ctrl Pts',(-18.778832216358,-4.28545098663153,0.));
#12616=CARTESIAN_POINT('Ctrl Pts',(-18.8219166495975,-4.30608591031525,
0.));
#12617=CARTESIAN_POINT('Ctrl Pts',(-18.8647973781745,-4.32737526247704,
0.));
#12618=CARTESIAN_POINT('Ctrl Pts',(-18.9074876952706,-4.34926881342021,
0.));
#12619=CARTESIAN_POINT('Ctrl Pts',(-18.9500107909187,-4.37168516143122,
0.));
#12620=CARTESIAN_POINT('Ctrl Pts',(-18.9923914823906,-4.39453820875554,
0.));
#12621=CARTESIAN_POINT('Ctrl Pts',(-19.034647328575,-4.41776558033331,0.));
#12622=CARTESIAN_POINT('Ctrl Pts',(-19.0767833717249,-4.44134542994081,
0.));
#12623=CARTESIAN_POINT('Ctrl Pts',(-19.1187970904933,-4.46528051067021,
0.));
#12624=CARTESIAN_POINT('Ctrl Pts',(-19.1606814968494,-4.48958819710576,
0.));
#12625=CARTESIAN_POINT('Ctrl Pts',(-19.2024287376926,-4.51428889122954,
0.));
#12626=CARTESIAN_POINT('Ctrl Pts',(-19.2440340196551,-4.53939338835151,
0.));
#12627=CARTESIAN_POINT('Ctrl Pts',(-19.2854975819105,-4.5648965160674,0.));
#12628=CARTESIAN_POINT('Ctrl Pts',(-19.3268225655679,-4.59078395765677,
0.));
#12629=CARTESIAN_POINT('Ctrl Pts',(-19.3680137353983,-4.61703633725711,
0.));
#12630=CARTESIAN_POINT('Ctrl Pts',(-19.4090759683639,-4.64363405547472,
0.));
#12631=CARTESIAN_POINT('Ctrl Pts',(-19.4500125912299,-4.67056260851453,
0.));
#12632=CARTESIAN_POINT('Ctrl Pts',(-19.4908246636763,-4.69781487613784,
0.));
#12633=CARTESIAN_POINT('Ctrl Pts',(-19.531511899192,-4.72538815796615,0.));
#12634=CARTESIAN_POINT('Ctrl Pts',(-19.5720732205813,-4.7532823819461,0.));
#12635=CARTESIAN_POINT('Ctrl Pts',(-19.6125074152527,-4.7814979936173,0.));
#12636=CARTESIAN_POINT('Ctrl Pts',(-19.6528138625329,-4.8100336141806,0.));
#12637=CARTESIAN_POINT('Ctrl Pts',(-19.6929928227072,-4.83888510708974,
0.));
#12638=CARTESIAN_POINT('Ctrl Pts',(-19.7330450480715,-4.86804682289086,
0.));
#12639=CARTESIAN_POINT('Ctrl Pts',(-19.772971552601,-4.89751233527804,0.));
#12640=CARTESIAN_POINT('Ctrl Pts',(-19.8127733387903,-4.92727531494346,
0.));
#12641=CARTESIAN_POINT('Ctrl Pts',(-19.8524510953961,-4.95733049830095,
0.));
#12642=CARTESIAN_POINT('Ctrl Pts',(-19.8920050831202,-4.98767405031333,
0.));
#12643=CARTESIAN_POINT('Ctrl Pts',(-19.931435301086,-5.01830302225557,0.));
#12644=CARTESIAN_POINT('Ctrl Pts',(-19.9707415879783,-5.04921502064063,
0.));
#12645=CARTESIAN_POINT('Ctrl Pts',(-20.0099237417205,-5.08040781745336,
0.));
#12646=CARTESIAN_POINT('Ctrl Pts',(-20.0489816528155,-5.11187891582334,
0.));
#12647=CARTESIAN_POINT('Ctrl Pts',(-20.087915358486,-5.14362537555397,0.));
#12648=CARTESIAN_POINT('Ctrl Pts',(-20.1267249732337,-5.17564404279921,
0.));
#12649=CARTESIAN_POINT('Ctrl Pts',(-20.1654106491899,-5.20793168386163,
0.));
#12650=CARTESIAN_POINT('Ctrl Pts',(-20.2039725283917,-5.2404851444189,0.));
#12651=CARTESIAN_POINT('Ctrl Pts',(-20.2424106921768,-5.2733015229815,0.));
#12652=CARTESIAN_POINT('Ctrl Pts',(-20.2807251380077,-5.30637824220997,
0.));
#12653=CARTESIAN_POINT('Ctrl Pts',(-20.3189158047642,-5.33971294212213,
0.));
#12654=CARTESIAN_POINT('Ctrl Pts',(-20.3569825877537,-5.37330341114649,
0.));
#12655=CARTESIAN_POINT('Ctrl Pts',(-20.3949253578015,-5.40714750595874,
0.));
#12656=CARTESIAN_POINT('Ctrl Pts',(-20.4327439816542,-5.44124306065111,
0.));
#12657=CARTESIAN_POINT('Ctrl Pts',(-20.4704383353718,-5.4755878444985,0.));
#12658=CARTESIAN_POINT('Ctrl Pts',(-20.5080083009242,-5.51017962306782,
0.));
#12659=CARTESIAN_POINT('Ctrl Pts',(-20.5454537676144,-5.5450161968946,0.));
#12660=CARTESIAN_POINT('Ctrl Pts',(-20.5827746317185,-5.58009544402474,
0.));
#12661=CARTESIAN_POINT('Ctrl Pts',(-20.6199707996366,-5.61541536715149,
0.));
#12662=CARTESIAN_POINT('Ctrl Pts',(-20.6570421847033,-5.65097411164334,
0.));
#12663=CARTESIAN_POINT('Ctrl Pts',(-20.6939886877061,-5.68676990500163,
0.));
#12664=CARTESIAN_POINT('Ctrl Pts',(-20.7308101804425,-5.72280100798241,
0.));
#12665=CARTESIAN_POINT('Ctrl Pts',(-20.7675064905026,-5.75906566327795,
0.));
#12666=CARTESIAN_POINT('Ctrl Pts',(-20.8040773827343,-5.79556203439644,
0.));
#12667=CARTESIAN_POINT('Ctrl Pts',(-20.8405225541277,-5.83228817460177,
0.));
#12668=CARTESIAN_POINT('Ctrl Pts',(-20.8768416821402,-5.86924212736287,
0.));
#12669=CARTESIAN_POINT('Ctrl Pts',(-20.9130344665641,-5.90642200662599,
0.));
#12670=CARTESIAN_POINT('Ctrl Pts',(-20.9491006734021,-5.94382608200804,
0.));
#12671=CARTESIAN_POINT('Ctrl Pts',(-20.9850401822713,-5.98145286361836,
0.));
#12672=CARTESIAN_POINT('Ctrl Pts',(-21.0280155918661,-6.02687083887286,
0.));
#12673=CARTESIAN_POINT('Ctrl Pts',(-21.0636702474951,-6.06499496148844,
0.));
#12674=CARTESIAN_POINT('Ctrl Pts',(-21.0920928984154,-6.09567013127871,
0.));
#12675=CARTESIAN_POINT('Ctrl Pts',(-21.1133530893457,-6.118775337615,0.));
#12676=CARTESIAN_POINT('Ctrl Pts',(-21.1275013067528,-6.1342227326009,0.));
#12677=CARTESIAN_POINT('Ctrl Pts',(-18.337935196262,-4.1144891981253,13.));
#12678=CARTESIAN_POINT('Ctrl Pts',(-18.3534360435645,-4.11796712887951,
13.));
#12679=CARTESIAN_POINT('Ctrl Pts',(-18.3688191548995,-4.12185943358937,
13.));
#12680=CARTESIAN_POINT('Ctrl Pts',(-18.3840926404824,-4.12613856044267,
13.));
#12681=CARTESIAN_POINT('Ctrl Pts',(-18.4019943079477,-4.13115401716693,
13.));
#12682=CARTESIAN_POINT('Ctrl Pts',(-18.4197456248295,-4.13670006307401,
13.));
#12683=CARTESIAN_POINT('Ctrl Pts',(-18.4373797424196,-4.1426637807957,13.));
#12684=CARTESIAN_POINT('Ctrl Pts',(-18.4621917897769,-4.15105501703309,
13.));
#12685=CARTESIAN_POINT('Ctrl Pts',(-18.4867739015683,-4.16026629328987,
13.));
#12686=CARTESIAN_POINT('Ctrl Pts',(-18.5112408492934,-4.16990400115282,
13.));
#12687=CARTESIAN_POINT('Ctrl Pts',(-18.5275152282609,-4.17631459686346,
13.));
#12688=CARTESIAN_POINT('Ctrl Pts',(-18.5437392096496,-4.18291190640786,
13.));
#12689=CARTESIAN_POINT('Ctrl Pts',(-18.5599376581358,-4.18960898617043,
13.));
#12690=CARTESIAN_POINT('Ctrl Pts',(-18.5769891804703,-4.19665876042785,
13.));
#12691=CARTESIAN_POINT('Ctrl Pts',(-18.5940126577989,-4.20381824254442,
13.));
#12692=CARTESIAN_POINT('Ctrl Pts',(-18.6110185062838,-4.21104759333806,
13.));
#12693=CARTESIAN_POINT('Ctrl Pts',(-18.6299044319376,-4.21907618313382,
13.));
#12694=CARTESIAN_POINT('Ctrl Pts',(-18.6487682283615,-4.22719219297435,
13.));
#12695=CARTESIAN_POINT('Ctrl Pts',(-18.6676042988365,-4.23540730606872,
13.));
#12696=CARTESIAN_POINT('Ctrl Pts',(-18.6960005893047,-4.24779198778706,
13.));
#12697=CARTESIAN_POINT('Ctrl Pts',(-18.7243319351566,-4.26040793123127,
13.));
#12698=CARTESIAN_POINT('Ctrl Pts',(-18.7525479285623,-4.27340283281641,
13.));
#12699=CARTESIAN_POINT('Ctrl Pts',(-18.7730462309054,-4.28284334471974,
13.));
#12700=CARTESIAN_POINT('Ctrl Pts',(-18.7934827312586,-4.29248702330122,
13.));
#12701=CARTESIAN_POINT('Ctrl Pts',(-18.8138501272238,-4.30235320731447,
13.));
#12702=CARTESIAN_POINT('Ctrl Pts',(-18.8387475247628,-4.31441377244467,
13.));
#12703=CARTESIAN_POINT('Ctrl Pts',(-18.8635420328974,-4.32680560862846,
13.));
#12704=CARTESIAN_POINT('Ctrl Pts',(-18.8882460103721,-4.33948253068856,
13.));
#12705=CARTESIAN_POINT('Ctrl Pts',(-18.9149304060727,-4.35317571045545,
13.));
#12706=CARTESIAN_POINT('Ctrl Pts',(-18.9415109549191,-4.36719580768733,
13.));
#12707=CARTESIAN_POINT('Ctrl Pts',(-18.9680129070824,-4.38145466528704,
13.));
#12708=CARTESIAN_POINT('Ctrl Pts',(-18.9924793848252,-4.39461837564137,
13.));
#12709=CARTESIAN_POINT('Ctrl Pts',(-19.0168796293529,-4.40798318219363,
13.));
#12710=CARTESIAN_POINT('Ctrl Pts',(-19.0412206988293,-4.42152146524019,
13.));
#12711=CARTESIAN_POINT('Ctrl Pts',(-19.0742892915424,-4.43991391790276,
13.));
#12712=CARTESIAN_POINT('Ctrl Pts',(-19.1072480696,-4.45862842583326,13.));
#12713=CARTESIAN_POINT('Ctrl Pts',(-19.1400849917464,-4.47769255669731,
13.));
#12714=CARTESIAN_POINT('Ctrl Pts',(-19.1717719124003,-4.49608903123077,
13.));
#12715=CARTESIAN_POINT('Ctrl Pts',(-19.2033430485145,-4.51481852753576,
13.));
#12716=CARTESIAN_POINT('Ctrl Pts',(-19.234791092488,-4.53389559694226,13.));
#12717=CARTESIAN_POINT('Ctrl Pts',(-19.2775141413934,-4.55981233026633,
13.));
#12718=CARTESIAN_POINT('Ctrl Pts',(-19.3200109594547,-4.58636743991277,
13.));
#12719=CARTESIAN_POINT('Ctrl Pts',(-19.3623013146402,-4.61347737193446,
13.));
#12720=CARTESIAN_POINT('Ctrl Pts',(-19.399473617434,-4.63730641279748,13.));
#12721=CARTESIAN_POINT('Ctrl Pts',(-19.4364884576265,-4.66155758403617,
13.));
#12722=CARTESIAN_POINT('Ctrl Pts',(-19.4733518508893,-4.68619912965976,
13.));
#12723=CARTESIAN_POINT('Ctrl Pts',(-19.5276974421966,-4.72252675034556,
13.));
#12724=CARTESIAN_POINT('Ctrl Pts',(-19.5817111528826,-4.7597114391696,13.));
#12725=CARTESIAN_POINT('Ctrl Pts',(-19.6353839065147,-4.79774570303518,
13.));
#12726=CARTESIAN_POINT('Ctrl Pts',(-19.7031194454445,-4.84574531524799,
13.));
#12727=CARTESIAN_POINT('Ctrl Pts',(-19.7703134647831,-4.8950930427256,13.));
#12728=CARTESIAN_POINT('Ctrl Pts',(-19.8369838018469,-4.94566457621167,
13.));
#12729=CARTESIAN_POINT('Ctrl Pts',(-19.9272939135678,-5.01416761729656,
13.));
#12730=CARTESIAN_POINT('Ctrl Pts',(-20.0166413602828,-5.08492180312729,
13.));
#12731=CARTESIAN_POINT('Ctrl Pts',(-20.1050225704216,-5.15778644838132,
13.));
#12732=CARTESIAN_POINT('Ctrl Pts',(-20.1838167338246,-5.22274718783514,
13.));
#12733=CARTESIAN_POINT('Ctrl Pts',(-20.2618454267474,-5.28937724234836,
13.));
#12734=CARTESIAN_POINT('Ctrl Pts',(-20.3391090332473,-5.35757729646381,
13.));
#12735=CARTESIAN_POINT('Ctrl Pts',(-20.4486128105791,-5.45423552765683,
13.));
#12736=CARTESIAN_POINT('Ctrl Pts',(-20.5565772409505,-5.55405241054101,
13.));
#12737=CARTESIAN_POINT('Ctrl Pts',(-20.6629906947268,-5.65680258421402,
13.));
#12738=CARTESIAN_POINT('Ctrl Pts',(-20.745650141592,-5.73661648198461,13.));
#12739=CARTESIAN_POINT('Ctrl Pts',(-20.8273750331781,-5.81820510936894,
13.));
#12740=CARTESIAN_POINT('Ctrl Pts',(-20.9081522158766,-5.90147459332601,
13.));
#12741=CARTESIAN_POINT('Ctrl Pts',(-20.9780305852213,-5.9735089916636,13.));
#12742=CARTESIAN_POINT('Ctrl Pts',(-21.0471984394024,-6.04679718721607,
13.));
#12743=CARTESIAN_POINT('Ctrl Pts',(-21.1156584437795,-6.12131239523347,
13.));
#12744=CARTESIAN_POINT('Ctrl Pts',(-21.11960842029,-6.12561174233439,13.));
#12745=CARTESIAN_POINT('Ctrl Pts',(-21.1235560412392,-6.12991518820048,
13.));
#12746=CARTESIAN_POINT('Ctrl Pts',(-21.1275013067528,-6.1342227326009,13.));
#12747=CARTESIAN_POINT('Ctrl Pts',(-21.9890268624765,-0.694764450219579,
0.));
#12748=CARTESIAN_POINT('Ctrl Pts',(-21.9890268624765,-0.694764450219579,
21.));
#12749=CARTESIAN_POINT('Ctrl Pts',(-21.9799122315157,-0.699924103234221,
0.));
#12750=CARTESIAN_POINT('Ctrl Pts',(-21.9799122315157,-0.699924103234221,
21.));
#12751=CARTESIAN_POINT('Ctrl Pts',(-21.9616777523685,-0.710218621843554,
0.));
#12752=CARTESIAN_POINT('Ctrl Pts',(-21.9616777523685,-0.710218621843554,
21.));
#12753=CARTESIAN_POINT('Ctrl Pts',(-21.9343103819749,-0.725586037496633,
0.));
#12754=CARTESIAN_POINT('Ctrl Pts',(-21.9343103819749,-0.725586037496633,
21.));
#12755=CARTESIAN_POINT('Ctrl Pts',(-21.8977892409997,-0.74592715110982,
0.));
#12756=CARTESIAN_POINT('Ctrl Pts',(-21.8977892409997,-0.74592715110982,
21.));
#12757=CARTESIAN_POINT('Ctrl Pts',(-21.8520856039249,-0.771105213258328,
0.));
#12758=CARTESIAN_POINT('Ctrl Pts',(-21.8520856039249,-0.771105213258328,
21.));
#12759=CARTESIAN_POINT('Ctrl Pts',(-21.8063297959755,-0.796034321106411,
0.));
#12760=CARTESIAN_POINT('Ctrl Pts',(-21.8063297959755,-0.796034321106411,
21.));
#12761=CARTESIAN_POINT('Ctrl Pts',(-21.7605219769118,-0.820713597934076,
0.));
#12762=CARTESIAN_POINT('Ctrl Pts',(-21.7605219769118,-0.820713597934076,
21.));
#12763=CARTESIAN_POINT('Ctrl Pts',(-21.7146624809285,-0.845141916726556,
0.));
#12764=CARTESIAN_POINT('Ctrl Pts',(-21.7146624809285,-0.845141916726556,
21.));
#12765=CARTESIAN_POINT('Ctrl Pts',(-21.6687518829182,-0.869317897714098,
0.));
#12766=CARTESIAN_POINT('Ctrl Pts',(-21.6687518829182,-0.869317897714098,
21.));
#12767=CARTESIAN_POINT('Ctrl Pts',(-21.6227909401433,-0.89323996751367,
0.));
#12768=CARTESIAN_POINT('Ctrl Pts',(-21.6227909401433,-0.89323996751367,
21.));
#12769=CARTESIAN_POINT('Ctrl Pts',(-21.5767805209408,-0.916906425150852,
0.));
#12770=CARTESIAN_POINT('Ctrl Pts',(-21.5767805209408,-0.916906425150852,
21.));
#12771=CARTESIAN_POINT('Ctrl Pts',(-21.5307215366685,-0.940315509525148,
0.));
#12772=CARTESIAN_POINT('Ctrl Pts',(-21.5307215366685,-0.940315509525148,
21.));
#12773=CARTESIAN_POINT('Ctrl Pts',(-21.4846148770804,-0.96346546281577,
0.));
#12774=CARTESIAN_POINT('Ctrl Pts',(-21.4846148770804,-0.96346546281577,
21.));
#12775=CARTESIAN_POINT('Ctrl Pts',(-21.4384613333266,-0.986354611081132,
0.));
#12776=CARTESIAN_POINT('Ctrl Pts',(-21.4384613333266,-0.986354611081132,
21.));
#12777=CARTESIAN_POINT('Ctrl Pts',(-21.3922616124166,-1.00898133629988,
0.));
#12778=CARTESIAN_POINT('Ctrl Pts',(-21.3922616124166,-1.00898133629988,
21.));
#12779=CARTESIAN_POINT('Ctrl Pts',(-21.3460163737343,-1.03134402396953,
0.));
#12780=CARTESIAN_POINT('Ctrl Pts',(-21.3460163737343,-1.03134402396953,
21.));
#12781=CARTESIAN_POINT('Ctrl Pts',(-21.2997262593683,-1.05344101900192,
0.));
#12782=CARTESIAN_POINT('Ctrl Pts',(-21.2997262593683,-1.05344101900192,
21.));
#12783=CARTESIAN_POINT('Ctrl Pts',(-21.2533919248553,-1.07527058431887,
0.));
#12784=CARTESIAN_POINT('Ctrl Pts',(-21.2533919248553,-1.07527058431887,
21.));
#12785=CARTESIAN_POINT('Ctrl Pts',(-21.2070140764156,-1.09683084929266,
0.));
#12786=CARTESIAN_POINT('Ctrl Pts',(-21.2070140764156,-1.09683084929266,
21.));
#12787=CARTESIAN_POINT('Ctrl Pts',(-21.1605934684164,-1.11811982787746,
0.));
#12788=CARTESIAN_POINT('Ctrl Pts',(-21.1605934684164,-1.11811982787746,
21.));
#12789=CARTESIAN_POINT('Ctrl Pts',(-21.1141308858087,-1.13913546246555,
0.));
#12790=CARTESIAN_POINT('Ctrl Pts',(-21.1141308858087,-1.13913546246555,
21.));
#12791=CARTESIAN_POINT('Ctrl Pts',(-21.0676271313238,-1.15987566445807,
0.));
#12792=CARTESIAN_POINT('Ctrl Pts',(-21.0676271313238,-1.15987566445807,
21.));
#12793=CARTESIAN_POINT('Ctrl Pts',(-21.0210830121673,-1.18033835060894,
0.));
#12794=CARTESIAN_POINT('Ctrl Pts',(-21.0210830121673,-1.18033835060894,
21.));
#12795=CARTESIAN_POINT('Ctrl Pts',(-20.9744993243732,-1.20052150219503,
0.));
#12796=CARTESIAN_POINT('Ctrl Pts',(-20.9744993243732,-1.20052150219503,
21.));
#12797=CARTESIAN_POINT('Ctrl Pts',(-20.9278768531175,-1.22042312071096,
0.));
#12798=CARTESIAN_POINT('Ctrl Pts',(-20.9278768531175,-1.22042312071096,
21.));
#12799=CARTESIAN_POINT('Ctrl Pts',(-20.881216381382,-1.24004113517905,0.));
#12800=CARTESIAN_POINT('Ctrl Pts',(-20.881216381382,-1.24004113517905,21.));
#12801=CARTESIAN_POINT('Ctrl Pts',(-20.83451869657,-1.25937332001005,0.));
#12802=CARTESIAN_POINT('Ctrl Pts',(-20.83451869657,-1.25937332001005,21.));
#12803=CARTESIAN_POINT('Ctrl Pts',(-20.7877845975367,-1.27841722479262,
0.));
#12804=CARTESIAN_POINT('Ctrl Pts',(-20.7877845975367,-1.27841722479262,
21.));
#12805=CARTESIAN_POINT('Ctrl Pts',(-20.7410149035348,-1.29717006491149,
0.));
#12806=CARTESIAN_POINT('Ctrl Pts',(-20.7410149035348,-1.29717006491149,
21.));
#12807=CARTESIAN_POINT('Ctrl Pts',(-20.694210454218,-1.31562879653596,0.));
#12808=CARTESIAN_POINT('Ctrl Pts',(-20.694210454218,-1.31562879653596,21.));
#12809=CARTESIAN_POINT('Ctrl Pts',(-20.6473721041685,-1.3337902972259,0.));
#12810=CARTESIAN_POINT('Ctrl Pts',(-20.6473721041685,-1.3337902972259,21.));
#12811=CARTESIAN_POINT('Ctrl Pts',(-20.6005007190809,-1.35165153211252,
0.));
#12812=CARTESIAN_POINT('Ctrl Pts',(-20.6005007190809,-1.35165153211252,
21.));
#12813=CARTESIAN_POINT('Ctrl Pts',(-20.5535971721246,-1.36920969340018,
0.));
#12814=CARTESIAN_POINT('Ctrl Pts',(-20.5535971721246,-1.36920969340018,
21.));
#12815=CARTESIAN_POINT('Ctrl Pts',(-20.5066623390132,-1.38646244026049,
0.));
#12816=CARTESIAN_POINT('Ctrl Pts',(-20.5066623390132,-1.38646244026049,
21.));
#12817=CARTESIAN_POINT('Ctrl Pts',(-20.4596971004275,-1.40340771617024,
0.));
#12818=CARTESIAN_POINT('Ctrl Pts',(-20.4596971004275,-1.40340771617024,
21.));
#12819=CARTESIAN_POINT('Ctrl Pts',(-20.4127023494155,-1.4200432946371,0.));
#12820=CARTESIAN_POINT('Ctrl Pts',(-20.4127023494155,-1.4200432946371,21.));
#12821=CARTESIAN_POINT('Ctrl Pts',(-20.3656789980171,-1.43636637152782,
0.));
#12822=CARTESIAN_POINT('Ctrl Pts',(-20.3656789980171,-1.43636637152782,
21.));
#12823=CARTESIAN_POINT('Ctrl Pts',(-20.3186279833818,-1.45237321894403,
0.));
#12824=CARTESIAN_POINT('Ctrl Pts',(-20.3186279833818,-1.45237321894403,
21.));
#12825=CARTESIAN_POINT('Ctrl Pts',(-20.2715502770004,-1.46805861808021,
0.));
#12826=CARTESIAN_POINT('Ctrl Pts',(-20.2715502770004,-1.46805861808021,
21.));
#12827=CARTESIAN_POINT('Ctrl Pts',(-20.224446881308,-1.48341623961913,0.));
#12828=CARTESIAN_POINT('Ctrl Pts',(-20.224446881308,-1.48341623961913,21.));
#12829=CARTESIAN_POINT('Ctrl Pts',(-20.1773188177942,-1.49843965844502,
0.));
#12830=CARTESIAN_POINT('Ctrl Pts',(-20.1773188177942,-1.49843965844502,
21.));
#12831=CARTESIAN_POINT('Ctrl Pts',(-20.1301671167606,-1.51312326913583,
0.));
#12832=CARTESIAN_POINT('Ctrl Pts',(-20.1301671167606,-1.51312326913583,
21.));
#12833=CARTESIAN_POINT('Ctrl Pts',(-20.0829928089241,-1.52746305716964,
0.));
#12834=CARTESIAN_POINT('Ctrl Pts',(-20.0829928089241,-1.52746305716964,
21.));
#12835=CARTESIAN_POINT('Ctrl Pts',(-20.0357969106526,-1.54145790302917,
0.));
#12836=CARTESIAN_POINT('Ctrl Pts',(-20.0357969106526,-1.54145790302917,
21.));
#12837=CARTESIAN_POINT('Ctrl Pts',(-19.9885804375097,-1.55510860515913,
0.));
#12838=CARTESIAN_POINT('Ctrl Pts',(-19.9885804375097,-1.55510860515913,
21.));
#12839=CARTESIAN_POINT('Ctrl Pts',(-19.9413444362352,-1.56841542790452,
0.));
#12840=CARTESIAN_POINT('Ctrl Pts',(-19.9413444362352,-1.56841542790452,
21.));
#12841=CARTESIAN_POINT('Ctrl Pts',(-19.8940900137801,-1.58137589158952,
0.));
#12842=CARTESIAN_POINT('Ctrl Pts',(-19.8940900137801,-1.58137589158952,
21.));
#12843=CARTESIAN_POINT('Ctrl Pts',(-19.8468183626037,-1.59398289700559,
0.));
#12844=CARTESIAN_POINT('Ctrl Pts',(-19.8468183626037,-1.59398289700559,
21.));
#12845=CARTESIAN_POINT('Ctrl Pts',(-19.7995308006834,-1.60622162219699,
0.));
#12846=CARTESIAN_POINT('Ctrl Pts',(-19.7995308006834,-1.60622162219699,
21.));
#12847=CARTESIAN_POINT('Ctrl Pts',(-19.7522287462982,-1.61807191996833,
0.));
#12848=CARTESIAN_POINT('Ctrl Pts',(-19.7522287462982,-1.61807191996833,
21.));
#12849=CARTESIAN_POINT('Ctrl Pts',(-19.7049136553525,-1.62951389038421,
0.));
#12850=CARTESIAN_POINT('Ctrl Pts',(-19.7049136553525,-1.62951389038421,
21.));
#12851=CARTESIAN_POINT('Ctrl Pts',(-19.6575869645839,-1.64053294677821,
0.));
#12852=CARTESIAN_POINT('Ctrl Pts',(-19.6575869645839,-1.64053294677821,
21.));
#12853=CARTESIAN_POINT('Ctrl Pts',(-19.6102500448855,-1.65112409599282,
0.));
#12854=CARTESIAN_POINT('Ctrl Pts',(-19.6102500448855,-1.65112409599282,
21.));
#12855=CARTESIAN_POINT('Ctrl Pts',(-19.5629041190868,-1.66129908621006,
0.));
#12856=CARTESIAN_POINT('Ctrl Pts',(-19.5629041190868,-1.66129908621006,
21.));
#12857=CARTESIAN_POINT('Ctrl Pts',(-19.5155503513712,-1.67107974760948,
0.));
#12858=CARTESIAN_POINT('Ctrl Pts',(-19.5155503513712,-1.67107974760948,
21.));
#12859=CARTESIAN_POINT('Ctrl Pts',(-19.4681900187091,-1.68048476382294,
0.));
#12860=CARTESIAN_POINT('Ctrl Pts',(-19.4681900187091,-1.68048476382294,
21.));
#12861=CARTESIAN_POINT('Ctrl Pts',(-19.4208246682917,-1.6895175323357,0.));
#12862=CARTESIAN_POINT('Ctrl Pts',(-19.4208246682917,-1.6895175323357,21.));
#12863=CARTESIAN_POINT('Ctrl Pts',(-19.3734562555057,-1.69815571801252,
0.));
#12864=CARTESIAN_POINT('Ctrl Pts',(-19.3734562555057,-1.69815571801252,
21.));
#12865=CARTESIAN_POINT('Ctrl Pts',(-19.3260873558094,-1.70633457265124,
0.));
#12866=CARTESIAN_POINT('Ctrl Pts',(-19.3260873558094,-1.70633457265124,
21.));
#12867=CARTESIAN_POINT('Ctrl Pts',(-19.2787209722437,-1.71396454346262,
0.));
#12868=CARTESIAN_POINT('Ctrl Pts',(-19.2787209722437,-1.71396454346262,
21.));
#12869=CARTESIAN_POINT('Ctrl Pts',(-19.2313602042899,-1.72096104670234,
0.));
#12870=CARTESIAN_POINT('Ctrl Pts',(-19.2313602042899,-1.72096104670234,
21.));
#12871=CARTESIAN_POINT('Ctrl Pts',(-19.1840079312107,-1.72727220327098,
0.));
#12872=CARTESIAN_POINT('Ctrl Pts',(-19.1840079312107,-1.72727220327098,
21.));
#12873=CARTESIAN_POINT('Ctrl Pts',(-19.1366665585833,-1.73290313712353,
0.));
#12874=CARTESIAN_POINT('Ctrl Pts',(-19.1366665585833,-1.73290313712353,
21.));
#12875=CARTESIAN_POINT('Ctrl Pts',(-19.0893375576541,-1.7379530116984,0.));
#12876=CARTESIAN_POINT('Ctrl Pts',(-19.0893375576541,-1.7379530116984,21.));
#12877=CARTESIAN_POINT('Ctrl Pts',(-19.0420224296189,-1.74256297552949,
0.));
#12878=CARTESIAN_POINT('Ctrl Pts',(-19.0420224296189,-1.74256297552949,
21.));
#12879=CARTESIAN_POINT('Ctrl Pts',(-18.9947239970259,-1.74684309825012,
0.));
#12880=CARTESIAN_POINT('Ctrl Pts',(-18.9947239970259,-1.74684309825012,
21.));
#12881=CARTESIAN_POINT('Ctrl Pts',(-18.947447637865,-1.75080409924533,0.));
#12882=CARTESIAN_POINT('Ctrl Pts',(-18.947447637865,-1.75080409924533,21.));
#12883=CARTESIAN_POINT('Ctrl Pts',(-18.9002024267872,-1.75429229572775,
0.));
#12884=CARTESIAN_POINT('Ctrl Pts',(-18.9002024267872,-1.75429229572775,
21.));
#12885=CARTESIAN_POINT('Ctrl Pts',(-18.8530026395886,-1.75690876962597,
0.));
#12886=CARTESIAN_POINT('Ctrl Pts',(-18.8530026395886,-1.75690876962597,
21.));
#12887=CARTESIAN_POINT('Ctrl Pts',(-18.8058650094753,-1.7581175236483,0.));
#12888=CARTESIAN_POINT('Ctrl Pts',(-18.8058650094753,-1.7581175236483,21.));
#12889=CARTESIAN_POINT('Ctrl Pts',(-18.7682173836138,-1.75752447968136,
0.));
#12890=CARTESIAN_POINT('Ctrl Pts',(-18.7682173836138,-1.75752447968136,
21.));
#12891=CARTESIAN_POINT('Ctrl Pts',(-18.7400222442427,-1.75601041697575,
0.));
#12892=CARTESIAN_POINT('Ctrl Pts',(-18.7400222442427,-1.75601041697575,
21.));
#12893=CARTESIAN_POINT('Ctrl Pts',(-18.7212441956871,-1.75450132833463,
0.));
#12894=CARTESIAN_POINT('Ctrl Pts',(-18.7212441956871,-1.75450132833463,
21.));
#12895=CARTESIAN_POINT('Ctrl Pts',(-18.7118598491961,-1.75362185428836,
0.));
#12896=CARTESIAN_POINT('Ctrl Pts',(-18.7118598491961,-1.75362185428836,
21.));
#12897=CARTESIAN_POINT('',(-21.9890268624765,-0.694764450219644,0.));
#12898=CARTESIAN_POINT('Ctrl Pts',(-18.7118598491961,-1.75362185428836,
0.));
#12899=CARTESIAN_POINT('Ctrl Pts',(-18.7212441956871,-1.75450132833463,
0.));
#12900=CARTESIAN_POINT('Ctrl Pts',(-18.7400222442427,-1.75601041697575,
0.));
#12901=CARTESIAN_POINT('Ctrl Pts',(-18.7682173836138,-1.75752447968136,
0.));
#12902=CARTESIAN_POINT('Ctrl Pts',(-18.8058650094753,-1.7581175236483,0.));
#12903=CARTESIAN_POINT('Ctrl Pts',(-18.8530026395886,-1.75690876962597,
0.));
#12904=CARTESIAN_POINT('Ctrl Pts',(-18.9002024267872,-1.75429229572775,
0.));
#12905=CARTESIAN_POINT('Ctrl Pts',(-18.947447637865,-1.75080409924533,0.));
#12906=CARTESIAN_POINT('Ctrl Pts',(-18.9947239970259,-1.74684309825012,
0.));
#12907=CARTESIAN_POINT('Ctrl Pts',(-19.0420224296189,-1.74256297552949,
0.));
#12908=CARTESIAN_POINT('Ctrl Pts',(-19.0893375576541,-1.7379530116984,0.));
#12909=CARTESIAN_POINT('Ctrl Pts',(-19.1366665585833,-1.73290313712353,
0.));
#12910=CARTESIAN_POINT('Ctrl Pts',(-19.1840079312107,-1.72727220327098,
0.));
#12911=CARTESIAN_POINT('Ctrl Pts',(-19.2313602042899,-1.72096104670234,
0.));
#12912=CARTESIAN_POINT('Ctrl Pts',(-19.2787209722437,-1.71396454346262,
0.));
#12913=CARTESIAN_POINT('Ctrl Pts',(-19.3260873558094,-1.70633457265124,
0.));
#12914=CARTESIAN_POINT('Ctrl Pts',(-19.3734562555057,-1.69815571801252,
0.));
#12915=CARTESIAN_POINT('Ctrl Pts',(-19.4208246682917,-1.6895175323357,0.));
#12916=CARTESIAN_POINT('Ctrl Pts',(-19.4681900187091,-1.68048476382294,
0.));
#12917=CARTESIAN_POINT('Ctrl Pts',(-19.5155503513712,-1.67107974760948,
0.));
#12918=CARTESIAN_POINT('Ctrl Pts',(-19.5629041190868,-1.66129908621006,
0.));
#12919=CARTESIAN_POINT('Ctrl Pts',(-19.6102500448855,-1.65112409599282,
0.));
#12920=CARTESIAN_POINT('Ctrl Pts',(-19.6575869645839,-1.64053294677821,
0.));
#12921=CARTESIAN_POINT('Ctrl Pts',(-19.7049136553525,-1.62951389038421,
0.));
#12922=CARTESIAN_POINT('Ctrl Pts',(-19.7522287462982,-1.61807191996833,
0.));
#12923=CARTESIAN_POINT('Ctrl Pts',(-19.7995308006834,-1.60622162219699,
0.));
#12924=CARTESIAN_POINT('Ctrl Pts',(-19.8468183626037,-1.59398289700559,
0.));
#12925=CARTESIAN_POINT('Ctrl Pts',(-19.8940900137801,-1.58137589158952,
0.));
#12926=CARTESIAN_POINT('Ctrl Pts',(-19.9413444362352,-1.56841542790452,
0.));
#12927=CARTESIAN_POINT('Ctrl Pts',(-19.9885804375097,-1.55510860515913,
0.));
#12928=CARTESIAN_POINT('Ctrl Pts',(-20.0357969106526,-1.54145790302917,
0.));
#12929=CARTESIAN_POINT('Ctrl Pts',(-20.0829928089241,-1.52746305716964,
0.));
#12930=CARTESIAN_POINT('Ctrl Pts',(-20.1301671167606,-1.51312326913583,
0.));
#12931=CARTESIAN_POINT('Ctrl Pts',(-20.1773188177942,-1.49843965844502,
0.));
#12932=CARTESIAN_POINT('Ctrl Pts',(-20.224446881308,-1.48341623961913,0.));
#12933=CARTESIAN_POINT('Ctrl Pts',(-20.2715502770004,-1.46805861808021,
0.));
#12934=CARTESIAN_POINT('Ctrl Pts',(-20.3186279833818,-1.45237321894403,
0.));
#12935=CARTESIAN_POINT('Ctrl Pts',(-20.3656789980171,-1.43636637152782,
0.));
#12936=CARTESIAN_POINT('Ctrl Pts',(-20.4127023494155,-1.4200432946371,0.));
#12937=CARTESIAN_POINT('Ctrl Pts',(-20.4596971004275,-1.40340771617024,
0.));
#12938=CARTESIAN_POINT('Ctrl Pts',(-20.5066623390132,-1.38646244026049,
0.));
#12939=CARTESIAN_POINT('Ctrl Pts',(-20.5535971721246,-1.36920969340018,
0.));
#12940=CARTESIAN_POINT('Ctrl Pts',(-20.6005007190809,-1.35165153211252,
0.));
#12941=CARTESIAN_POINT('Ctrl Pts',(-20.6473721041685,-1.3337902972259,0.));
#12942=CARTESIAN_POINT('Ctrl Pts',(-20.694210454218,-1.31562879653596,0.));
#12943=CARTESIAN_POINT('Ctrl Pts',(-20.7410149035348,-1.29717006491149,
0.));
#12944=CARTESIAN_POINT('Ctrl Pts',(-20.7877845975367,-1.27841722479262,
0.));
#12945=CARTESIAN_POINT('Ctrl Pts',(-20.83451869657,-1.25937332001005,0.));
#12946=CARTESIAN_POINT('Ctrl Pts',(-20.881216381382,-1.24004113517905,0.));
#12947=CARTESIAN_POINT('Ctrl Pts',(-20.9278768531175,-1.22042312071096,
0.));
#12948=CARTESIAN_POINT('Ctrl Pts',(-20.9744993243732,-1.20052150219503,
0.));
#12949=CARTESIAN_POINT('Ctrl Pts',(-21.0210830121673,-1.18033835060894,
0.));
#12950=CARTESIAN_POINT('Ctrl Pts',(-21.0676271313238,-1.15987566445807,
0.));
#12951=CARTESIAN_POINT('Ctrl Pts',(-21.1141308858087,-1.13913546246555,
0.));
#12952=CARTESIAN_POINT('Ctrl Pts',(-21.1605934684164,-1.11811982787746,
0.));
#12953=CARTESIAN_POINT('Ctrl Pts',(-21.2070140764156,-1.09683084929266,
0.));
#12954=CARTESIAN_POINT('Ctrl Pts',(-21.2533919248553,-1.07527058431887,
0.));
#12955=CARTESIAN_POINT('Ctrl Pts',(-21.2997262593683,-1.05344101900192,
0.));
#12956=CARTESIAN_POINT('Ctrl Pts',(-21.3460163737343,-1.03134402396953,
0.));
#12957=CARTESIAN_POINT('Ctrl Pts',(-21.3922616124166,-1.00898133629988,
0.));
#12958=CARTESIAN_POINT('Ctrl Pts',(-21.4384613333266,-0.986354611081132,
0.));
#12959=CARTESIAN_POINT('Ctrl Pts',(-21.4846148770804,-0.96346546281577,
0.));
#12960=CARTESIAN_POINT('Ctrl Pts',(-21.5307215366685,-0.940315509525148,
0.));
#12961=CARTESIAN_POINT('Ctrl Pts',(-21.5767805209408,-0.916906425150852,
0.));
#12962=CARTESIAN_POINT('Ctrl Pts',(-21.6227909401433,-0.89323996751367,
0.));
#12963=CARTESIAN_POINT('Ctrl Pts',(-21.6687518829182,-0.869317897714098,
0.));
#12964=CARTESIAN_POINT('Ctrl Pts',(-21.7146624809285,-0.845141916726556,
0.));
#12965=CARTESIAN_POINT('Ctrl Pts',(-21.7605219769118,-0.820713597934076,
0.));
#12966=CARTESIAN_POINT('Ctrl Pts',(-21.8063297959755,-0.796034321106411,
0.));
#12967=CARTESIAN_POINT('Ctrl Pts',(-21.8612367655148,-0.766119391688711,
0.));
#12968=CARTESIAN_POINT('Ctrl Pts',(-21.9069273598709,-0.740879090965097,
0.));
#12969=CARTESIAN_POINT('Ctrl Pts',(-21.9434380560096,-0.720488353007145,
0.));
#12970=CARTESIAN_POINT('Ctrl Pts',(-21.970797600548,-0.705083756261758,
0.));
#12971=CARTESIAN_POINT('Ctrl Pts',(-21.9890268624765,-0.694764450219579,
0.));
#12972=CARTESIAN_POINT('',(-21.9890268624765,-0.694764450219644,13.));
#12973=CARTESIAN_POINT('Ctrl Pts',(-21.9890268624765,-0.694764450219579,
13.));
#12974=CARTESIAN_POINT('Ctrl Pts',(-21.8992923153509,-0.745561803243044,
13.));
#12975=CARTESIAN_POINT('Ctrl Pts',(-21.8092529632209,-0.794921865486053,
13.));
#12976=CARTESIAN_POINT('Ctrl Pts',(-21.71891375393,-0.84281926080538,13.));
#12977=CARTESIAN_POINT('Ctrl Pts',(-21.5692177628774,-0.92218732388059,
13.));
#12978=CARTESIAN_POINT('Ctrl Pts',(-21.418707272962,-0.997528955318343,
13.));
#12979=CARTESIAN_POINT('Ctrl Pts',(-21.267502258671,-1.06858105378788,13.));
#12980=CARTESIAN_POINT('Ctrl Pts',(-21.1512772179881,-1.12319586318391,
13.));
#12981=CARTESIAN_POINT('Ctrl Pts',(-21.034639156117,-1.17527598651002,13.));
#12982=CARTESIAN_POINT('Ctrl Pts',(-20.9176442431412,-1.22467603846418,
13.));
#12983=CARTESIAN_POINT('Ctrl Pts',(-20.7917020383065,-1.27785400410231,
13.));
#12984=CARTESIAN_POINT('Ctrl Pts',(-20.6653453745879,-1.32793259657608,
13.));
#12985=CARTESIAN_POINT('Ctrl Pts',(-20.5386490834973,-1.37465955678759,
13.));
#12986=CARTESIAN_POINT('Ctrl Pts',(-20.468506575479,-1.40052887113839,13.));
#12987=CARTESIAN_POINT('Ctrl Pts',(-20.3982600584712,-1.42537603682711,
13.));
#12988=CARTESIAN_POINT('Ctrl Pts',(-20.3279233191933,-1.44915458797959,
13.));
#12989=CARTESIAN_POINT('Ctrl Pts',(-20.2601440769455,-1.4720685330304,13.));
#12990=CARTESIAN_POINT('Ctrl Pts',(-20.1922811204785,-1.49398338578919,
13.));
#12991=CARTESIAN_POINT('Ctrl Pts',(-20.1243481778791,-1.51482335733726,
13.));
#12992=CARTESIAN_POINT('Ctrl Pts',(-20.0656332826906,-1.53283548368357,
13.));
#12993=CARTESIAN_POINT('Ctrl Pts',(-20.0068660712063,-1.55004791451012,
13.));
#12994=CARTESIAN_POINT('Ctrl Pts',(-19.9480555830993,-1.56645839157978,
13.));
#12995=CARTESIAN_POINT('Ctrl Pts',(-19.9058499566848,-1.5782354484752,13.));
#12996=CARTESIAN_POINT('Ctrl Pts',(-19.8636220199286,-1.58960230240354,
13.));
#12997=CARTESIAN_POINT('Ctrl Pts',(-19.8213758739716,-1.60051957233219,
13.));
#12998=CARTESIAN_POINT('Ctrl Pts',(-19.7798176538137,-1.61125906813568,
13.));
#12999=CARTESIAN_POINT('Ctrl Pts',(-19.7382418843902,-1.62155711742552,
13.));
#13000=CARTESIAN_POINT('Ctrl Pts',(-19.6966529616191,-1.63136143481693,
13.));
#13001=CARTESIAN_POINT('Ctrl Pts',(-19.6605929223136,-1.63986235397861,
13.));
#13002=CARTESIAN_POINT('Ctrl Pts',(-19.6245230263165,-1.6479896124833,13.));
#13003=CARTESIAN_POINT('Ctrl Pts',(-19.588445788193,-1.65575861448984,13.));
#13004=CARTESIAN_POINT('Ctrl Pts',(-19.5557680878316,-1.66279554782735,
13.));
#13005=CARTESIAN_POINT('Ctrl Pts',(-19.5230842951978,-1.66954412484817,
13.));
#13006=CARTESIAN_POINT('Ctrl Pts',(-19.4903963525255,-1.67602787924388,
13.));
#13007=CARTESIAN_POINT('Ctrl Pts',(-19.4628617563019,-1.68148945145379,
13.));
#13008=CARTESIAN_POINT('Ctrl Pts',(-19.4353241965609,-1.68676485594434,
13.));
#13009=CARTESIAN_POINT('Ctrl Pts',(-19.4077853966265,-1.69183425664604,
13.));
#13010=CARTESIAN_POINT('Ctrl Pts',(-19.3679337568149,-1.69917023102786,
13.));
#13011=CARTESIAN_POINT('Ctrl Pts',(-19.3280794804597,-1.70607400304717,
13.));
#13012=CARTESIAN_POINT('Ctrl Pts',(-19.2882303926777,-1.71232694125142,
13.));
#13013=CARTESIAN_POINT('Ctrl Pts',(-19.2641520278646,-1.71610520910184,
13.));
#13014=CARTESIAN_POINT('Ctrl Pts',(-19.2400756158948,-1.71964237036002,
13.));
#13015=CARTESIAN_POINT('Ctrl Pts',(-19.2160028184539,-1.72291205967493,
13.));
#13016=CARTESIAN_POINT('Ctrl Pts',(-19.1938009271133,-1.72592763304422,
13.));
#13017=CARTESIAN_POINT('Ctrl Pts',(-19.1716021268411,-1.72871436967926,
13.));
#13018=CARTESIAN_POINT('Ctrl Pts',(-19.1494073129248,-1.73129733452527,
13.));
#13019=CARTESIAN_POINT('Ctrl Pts',(-19.1188760970926,-1.73485046443652,
13.));
#13020=CARTESIAN_POINT('Ctrl Pts',(-19.088352219871,-1.73802530995722,13.));
#13021=CARTESIAN_POINT('Ctrl Pts',(-19.0578380259668,-1.74097263877159,
13.));
#13022=CARTESIAN_POINT('Ctrl Pts',(-19.0384792770416,-1.7428424767459,13.));
#13023=CARTESIAN_POINT('Ctrl Pts',(-19.0191244315082,-1.74462241724484,
13.));
#13024=CARTESIAN_POINT('Ctrl Pts',(-18.9997750006257,-1.74632097576469,
13.));
#13025=CARTESIAN_POINT('Ctrl Pts',(-18.9824097870453,-1.74784535297533,
13.));
#13026=CARTESIAN_POINT('Ctrl Pts',(-18.9650489251871,-1.74930491162087,
13.));
#13027=CARTESIAN_POINT('Ctrl Pts',(-18.9476944343333,-1.75066513119922,
13.));
#13028=CARTESIAN_POINT('Ctrl Pts',(-18.9294514080863,-1.75209499288047,
13.));
#13029=CARTESIAN_POINT('Ctrl Pts',(-18.911215425824,-1.75341524153972,13.));
#13030=CARTESIAN_POINT('Ctrl Pts',(-18.8929901413936,-1.75452347865236,
13.));
#13031=CARTESIAN_POINT('Ctrl Pts',(-18.8627179842862,-1.75636425804397,
13.));
#13032=CARTESIAN_POINT('Ctrl Pts',(-18.8324756678072,-1.75761169393937,
13.));
#13033=CARTESIAN_POINT('Ctrl Pts',(-18.8022820949953,-1.75764008468141,
13.));
#13034=CARTESIAN_POINT('Ctrl Pts',(-18.7856322843766,-1.75765574034698,
13.));
#13035=CARTESIAN_POINT('Ctrl Pts',(-18.7689972916915,-1.75729933637064,
13.));
#13036=CARTESIAN_POINT('Ctrl Pts',(-18.7523793043893,-1.75649392367919,
13.));
#13037=CARTESIAN_POINT('Ctrl Pts',(-18.7388614288228,-1.75583876199536,
13.));
#13038=CARTESIAN_POINT('Ctrl Pts',(-18.7253548001813,-1.75488656240187,
13.));
#13039=CARTESIAN_POINT('Ctrl Pts',(-18.7118598491961,-1.75362185428836,
13.));
#13040=CARTESIAN_POINT('',(-21.9890268624765,-0.694764450219644,0.));
#13041=CARTESIAN_POINT('Origin',(-5.6665783176868E-12,2.52435489670724E-28,
0.));
#13042=CARTESIAN_POINT('',(-21.9890268624765,0.694764450219584,0.));
#13043=CARTESIAN_POINT('Origin',(-5.6665783176868E-12,2.52435489670724E-28,
0.));
#13044=CARTESIAN_POINT('',(-21.9890268624765,0.694764450219584,13.));
#13045=CARTESIAN_POINT('Origin',(-5.6665783176868E-12,2.52435489670724E-28,
13.));
#13046=CARTESIAN_POINT('',(-21.9890268624765,0.694764450219584,0.));
#13047=CARTESIAN_POINT('Ctrl Pts',(-18.7118598491961,1.75362185428837,0.));
#13048=CARTESIAN_POINT('Ctrl Pts',(-18.7118598491961,1.75362185428837,21.));
#13049=CARTESIAN_POINT('Ctrl Pts',(-18.7212441956871,1.75450132833464,0.));
#13050=CARTESIAN_POINT('Ctrl Pts',(-18.7212441956871,1.75450132833464,21.));
#13051=CARTESIAN_POINT('Ctrl Pts',(-18.7400222442427,1.75601041697575,0.));
#13052=CARTESIAN_POINT('Ctrl Pts',(-18.7400222442427,1.75601041697575,21.));
#13053=CARTESIAN_POINT('Ctrl Pts',(-18.7682173836138,1.75752447968136,0.));
#13054=CARTESIAN_POINT('Ctrl Pts',(-18.7682173836138,1.75752447968136,21.));
#13055=CARTESIAN_POINT('Ctrl Pts',(-18.8058650094753,1.7581175236483,0.));
#13056=CARTESIAN_POINT('Ctrl Pts',(-18.8058650094753,1.7581175236483,21.));
#13057=CARTESIAN_POINT('Ctrl Pts',(-18.8530026395886,1.75690876962598,0.));
#13058=CARTESIAN_POINT('Ctrl Pts',(-18.8530026395886,1.75690876962598,21.));
#13059=CARTESIAN_POINT('Ctrl Pts',(-18.9002024267872,1.75429229572775,0.));
#13060=CARTESIAN_POINT('Ctrl Pts',(-18.9002024267872,1.75429229572775,21.));
#13061=CARTESIAN_POINT('Ctrl Pts',(-18.947447637865,1.75080409924533,0.));
#13062=CARTESIAN_POINT('Ctrl Pts',(-18.947447637865,1.75080409924533,21.));
#13063=CARTESIAN_POINT('Ctrl Pts',(-18.9947239970259,1.74684309825012,0.));
#13064=CARTESIAN_POINT('Ctrl Pts',(-18.9947239970259,1.74684309825012,21.));
#13065=CARTESIAN_POINT('Ctrl Pts',(-19.0420224296189,1.74256297552949,0.));
#13066=CARTESIAN_POINT('Ctrl Pts',(-19.0420224296189,1.74256297552949,21.));
#13067=CARTESIAN_POINT('Ctrl Pts',(-19.0893375576541,1.73795301169841,0.));
#13068=CARTESIAN_POINT('Ctrl Pts',(-19.0893375576541,1.73795301169841,21.));
#13069=CARTESIAN_POINT('Ctrl Pts',(-19.1366665585833,1.73290313712354,0.));
#13070=CARTESIAN_POINT('Ctrl Pts',(-19.1366665585833,1.73290313712354,21.));
#13071=CARTESIAN_POINT('Ctrl Pts',(-19.1840079312107,1.72727220327098,0.));
#13072=CARTESIAN_POINT('Ctrl Pts',(-19.1840079312107,1.72727220327098,21.));
#13073=CARTESIAN_POINT('Ctrl Pts',(-19.2313602042899,1.72096104670234,0.));
#13074=CARTESIAN_POINT('Ctrl Pts',(-19.2313602042899,1.72096104670234,21.));
#13075=CARTESIAN_POINT('Ctrl Pts',(-19.2787209722437,1.71396454346262,0.));
#13076=CARTESIAN_POINT('Ctrl Pts',(-19.2787209722437,1.71396454346262,21.));
#13077=CARTESIAN_POINT('Ctrl Pts',(-19.3260873558094,1.70633457265124,0.));
#13078=CARTESIAN_POINT('Ctrl Pts',(-19.3260873558094,1.70633457265124,21.));
#13079=CARTESIAN_POINT('Ctrl Pts',(-19.3734562555057,1.69815571801252,0.));
#13080=CARTESIAN_POINT('Ctrl Pts',(-19.3734562555057,1.69815571801252,21.));
#13081=CARTESIAN_POINT('Ctrl Pts',(-19.4208246682917,1.68951753233571,0.));
#13082=CARTESIAN_POINT('Ctrl Pts',(-19.4208246682917,1.68951753233571,21.));
#13083=CARTESIAN_POINT('Ctrl Pts',(-19.4681900187091,1.68048476382294,0.));
#13084=CARTESIAN_POINT('Ctrl Pts',(-19.4681900187091,1.68048476382294,21.));
#13085=CARTESIAN_POINT('Ctrl Pts',(-19.5155503513712,1.67107974760949,0.));
#13086=CARTESIAN_POINT('Ctrl Pts',(-19.5155503513712,1.67107974760949,21.));
#13087=CARTESIAN_POINT('Ctrl Pts',(-19.5629041190868,1.66129908621006,0.));
#13088=CARTESIAN_POINT('Ctrl Pts',(-19.5629041190868,1.66129908621006,21.));
#13089=CARTESIAN_POINT('Ctrl Pts',(-19.6102500448855,1.65112409599283,0.));
#13090=CARTESIAN_POINT('Ctrl Pts',(-19.6102500448855,1.65112409599283,21.));
#13091=CARTESIAN_POINT('Ctrl Pts',(-19.6575869645839,1.64053294677822,0.));
#13092=CARTESIAN_POINT('Ctrl Pts',(-19.6575869645839,1.64053294677822,21.));
#13093=CARTESIAN_POINT('Ctrl Pts',(-19.7049136553525,1.62951389038422,0.));
#13094=CARTESIAN_POINT('Ctrl Pts',(-19.7049136553525,1.62951389038422,21.));
#13095=CARTESIAN_POINT('Ctrl Pts',(-19.7522287462982,1.61807191996834,0.));
#13096=CARTESIAN_POINT('Ctrl Pts',(-19.7522287462982,1.61807191996834,21.));
#13097=CARTESIAN_POINT('Ctrl Pts',(-19.7995308006834,1.60622162219699,0.));
#13098=CARTESIAN_POINT('Ctrl Pts',(-19.7995308006834,1.60622162219699,21.));
#13099=CARTESIAN_POINT('Ctrl Pts',(-19.8468183626037,1.59398289700559,0.));
#13100=CARTESIAN_POINT('Ctrl Pts',(-19.8468183626037,1.59398289700559,21.));
#13101=CARTESIAN_POINT('Ctrl Pts',(-19.8940900137801,1.58137589158952,0.));
#13102=CARTESIAN_POINT('Ctrl Pts',(-19.8940900137801,1.58137589158952,21.));
#13103=CARTESIAN_POINT('Ctrl Pts',(-19.9413444362352,1.56841542790453,0.));
#13104=CARTESIAN_POINT('Ctrl Pts',(-19.9413444362352,1.56841542790453,21.));
#13105=CARTESIAN_POINT('Ctrl Pts',(-19.9885804375097,1.55510860515914,0.));
#13106=CARTESIAN_POINT('Ctrl Pts',(-19.9885804375097,1.55510860515914,21.));
#13107=CARTESIAN_POINT('Ctrl Pts',(-20.0357969106526,1.54145790302918,0.));
#13108=CARTESIAN_POINT('Ctrl Pts',(-20.0357969106526,1.54145790302918,21.));
#13109=CARTESIAN_POINT('Ctrl Pts',(-20.0829928089241,1.52746305716964,0.));
#13110=CARTESIAN_POINT('Ctrl Pts',(-20.0829928089241,1.52746305716964,21.));
#13111=CARTESIAN_POINT('Ctrl Pts',(-20.1301671167606,1.51312326913583,0.));
#13112=CARTESIAN_POINT('Ctrl Pts',(-20.1301671167606,1.51312326913583,21.));
#13113=CARTESIAN_POINT('Ctrl Pts',(-20.1773188177942,1.49843965844502,0.));
#13114=CARTESIAN_POINT('Ctrl Pts',(-20.1773188177942,1.49843965844502,21.));
#13115=CARTESIAN_POINT('Ctrl Pts',(-20.224446881308,1.48341623961914,0.));
#13116=CARTESIAN_POINT('Ctrl Pts',(-20.224446881308,1.48341623961914,21.));
#13117=CARTESIAN_POINT('Ctrl Pts',(-20.2715502770004,1.46805861808021,0.));
#13118=CARTESIAN_POINT('Ctrl Pts',(-20.2715502770004,1.46805861808021,21.));
#13119=CARTESIAN_POINT('Ctrl Pts',(-20.3186279833818,1.45237321894404,0.));
#13120=CARTESIAN_POINT('Ctrl Pts',(-20.3186279833818,1.45237321894404,21.));
#13121=CARTESIAN_POINT('Ctrl Pts',(-20.3656789980171,1.43636637152782,0.));
#13122=CARTESIAN_POINT('Ctrl Pts',(-20.3656789980171,1.43636637152782,21.));
#13123=CARTESIAN_POINT('Ctrl Pts',(-20.4127023494155,1.4200432946371,0.));
#13124=CARTESIAN_POINT('Ctrl Pts',(-20.4127023494155,1.4200432946371,21.));
#13125=CARTESIAN_POINT('Ctrl Pts',(-20.4596971004275,1.40340771617025,0.));
#13126=CARTESIAN_POINT('Ctrl Pts',(-20.4596971004275,1.40340771617025,21.));
#13127=CARTESIAN_POINT('Ctrl Pts',(-20.5066623390132,1.38646244026049,0.));
#13128=CARTESIAN_POINT('Ctrl Pts',(-20.5066623390132,1.38646244026049,21.));
#13129=CARTESIAN_POINT('Ctrl Pts',(-20.5535971721246,1.36920969340018,0.));
#13130=CARTESIAN_POINT('Ctrl Pts',(-20.5535971721246,1.36920969340018,21.));
#13131=CARTESIAN_POINT('Ctrl Pts',(-20.6005007190809,1.35165153211253,0.));
#13132=CARTESIAN_POINT('Ctrl Pts',(-20.6005007190809,1.35165153211253,21.));
#13133=CARTESIAN_POINT('Ctrl Pts',(-20.6473721041685,1.33379029722591,0.));
#13134=CARTESIAN_POINT('Ctrl Pts',(-20.6473721041685,1.33379029722591,21.));
#13135=CARTESIAN_POINT('Ctrl Pts',(-20.694210454218,1.31562879653596,0.));
#13136=CARTESIAN_POINT('Ctrl Pts',(-20.694210454218,1.31562879653596,21.));
#13137=CARTESIAN_POINT('Ctrl Pts',(-20.7410149035348,1.2971700649115,0.));
#13138=CARTESIAN_POINT('Ctrl Pts',(-20.7410149035348,1.2971700649115,21.));
#13139=CARTESIAN_POINT('Ctrl Pts',(-20.7877845975367,1.27841722479262,0.));
#13140=CARTESIAN_POINT('Ctrl Pts',(-20.7877845975367,1.27841722479262,21.));
#13141=CARTESIAN_POINT('Ctrl Pts',(-20.83451869657,1.25937332001005,0.));
#13142=CARTESIAN_POINT('Ctrl Pts',(-20.83451869657,1.25937332001005,21.));
#13143=CARTESIAN_POINT('Ctrl Pts',(-20.881216381382,1.24004113517905,0.));
#13144=CARTESIAN_POINT('Ctrl Pts',(-20.881216381382,1.24004113517905,21.));
#13145=CARTESIAN_POINT('Ctrl Pts',(-20.9278768531175,1.22042312071096,0.));
#13146=CARTESIAN_POINT('Ctrl Pts',(-20.9278768531175,1.22042312071096,21.));
#13147=CARTESIAN_POINT('Ctrl Pts',(-20.9744993243732,1.20052150219503,0.));
#13148=CARTESIAN_POINT('Ctrl Pts',(-20.9744993243732,1.20052150219503,21.));
#13149=CARTESIAN_POINT('Ctrl Pts',(-21.0210830121673,1.18033835060894,0.));
#13150=CARTESIAN_POINT('Ctrl Pts',(-21.0210830121673,1.18033835060894,21.));
#13151=CARTESIAN_POINT('Ctrl Pts',(-21.0676271313238,1.15987566445807,0.));
#13152=CARTESIAN_POINT('Ctrl Pts',(-21.0676271313238,1.15987566445807,21.));
#13153=CARTESIAN_POINT('Ctrl Pts',(-21.1141308858087,1.13913546246555,0.));
#13154=CARTESIAN_POINT('Ctrl Pts',(-21.1141308858087,1.13913546246555,21.));
#13155=CARTESIAN_POINT('Ctrl Pts',(-21.1605934684164,1.11811982787747,0.));
#13156=CARTESIAN_POINT('Ctrl Pts',(-21.1605934684164,1.11811982787747,21.));
#13157=CARTESIAN_POINT('Ctrl Pts',(-21.2070140764156,1.09683084929266,0.));
#13158=CARTESIAN_POINT('Ctrl Pts',(-21.2070140764156,1.09683084929266,21.));
#13159=CARTESIAN_POINT('Ctrl Pts',(-21.2533919248553,1.07527058431887,0.));
#13160=CARTESIAN_POINT('Ctrl Pts',(-21.2533919248553,1.07527058431887,21.));
#13161=CARTESIAN_POINT('Ctrl Pts',(-21.2997262593683,1.05344101900192,0.));
#13162=CARTESIAN_POINT('Ctrl Pts',(-21.2997262593683,1.05344101900192,21.));
#13163=CARTESIAN_POINT('Ctrl Pts',(-21.3460163737343,1.03134402396953,0.));
#13164=CARTESIAN_POINT('Ctrl Pts',(-21.3460163737343,1.03134402396953,21.));
#13165=CARTESIAN_POINT('Ctrl Pts',(-21.3922616124166,1.00898133629988,0.));
#13166=CARTESIAN_POINT('Ctrl Pts',(-21.3922616124166,1.00898133629988,21.));
#13167=CARTESIAN_POINT('Ctrl Pts',(-21.4384613333266,0.986354611081137,
0.));
#13168=CARTESIAN_POINT('Ctrl Pts',(-21.4384613333266,0.986354611081137,
21.));
#13169=CARTESIAN_POINT('Ctrl Pts',(-21.4846148770804,0.963465462815773,
0.));
#13170=CARTESIAN_POINT('Ctrl Pts',(-21.4846148770804,0.963465462815773,
21.));
#13171=CARTESIAN_POINT('Ctrl Pts',(-21.5307215366685,0.940315509525154,
0.));
#13172=CARTESIAN_POINT('Ctrl Pts',(-21.5307215366685,0.940315509525154,
21.));
#13173=CARTESIAN_POINT('Ctrl Pts',(-21.5767805209408,0.916906425150856,
0.));
#13174=CARTESIAN_POINT('Ctrl Pts',(-21.5767805209408,0.916906425150856,
21.));
#13175=CARTESIAN_POINT('Ctrl Pts',(-21.6227909401433,0.893239967513676,
0.));
#13176=CARTESIAN_POINT('Ctrl Pts',(-21.6227909401433,0.893239967513676,
21.));
#13177=CARTESIAN_POINT('Ctrl Pts',(-21.6687518829182,0.869317897714101,
0.));
#13178=CARTESIAN_POINT('Ctrl Pts',(-21.6687518829182,0.869317897714101,
21.));
#13179=CARTESIAN_POINT('Ctrl Pts',(-21.7146624809285,0.845141916726562,
0.));
#13180=CARTESIAN_POINT('Ctrl Pts',(-21.7146624809285,0.845141916726562,
21.));
#13181=CARTESIAN_POINT('Ctrl Pts',(-21.7605219769118,0.82071359793408,0.));
#13182=CARTESIAN_POINT('Ctrl Pts',(-21.7605219769118,0.82071359793408,21.));
#13183=CARTESIAN_POINT('Ctrl Pts',(-21.8063297959755,0.796034321106415,
0.));
#13184=CARTESIAN_POINT('Ctrl Pts',(-21.8063297959755,0.796034321106415,
21.));
#13185=CARTESIAN_POINT('Ctrl Pts',(-21.8520856039249,0.771105213258334,
0.));
#13186=CARTESIAN_POINT('Ctrl Pts',(-21.8520856039249,0.771105213258334,
21.));
#13187=CARTESIAN_POINT('Ctrl Pts',(-21.8977892409997,0.745927151109823,
0.));
#13188=CARTESIAN_POINT('Ctrl Pts',(-21.8977892409997,0.745927151109823,
21.));
#13189=CARTESIAN_POINT('Ctrl Pts',(-21.9343103819749,0.725586037496639,
0.));
#13190=CARTESIAN_POINT('Ctrl Pts',(-21.9343103819749,0.725586037496639,
21.));
#13191=CARTESIAN_POINT('Ctrl Pts',(-21.9616777523685,0.71021862184356,0.));
#13192=CARTESIAN_POINT('Ctrl Pts',(-21.9616777523685,0.71021862184356,21.));
#13193=CARTESIAN_POINT('Ctrl Pts',(-21.9799122315157,0.699924103234225,
0.));
#13194=CARTESIAN_POINT('Ctrl Pts',(-21.9799122315157,0.699924103234225,
21.));
#13195=CARTESIAN_POINT('Ctrl Pts',(-21.9890268624765,0.694764450219583,
0.));
#13196=CARTESIAN_POINT('Ctrl Pts',(-21.9890268624765,0.694764450219583,
21.));
#13197=CARTESIAN_POINT('Ctrl Pts',(-18.7118598491961,1.75362185428837,0.));
#13198=CARTESIAN_POINT('Ctrl Pts',(-18.7212441956871,1.75450132833464,0.));
#13199=CARTESIAN_POINT('Ctrl Pts',(-18.7400222442427,1.75601041697575,0.));
#13200=CARTESIAN_POINT('Ctrl Pts',(-18.7682173836138,1.75752447968136,0.));
#13201=CARTESIAN_POINT('Ctrl Pts',(-18.8058650094753,1.7581175236483,0.));
#13202=CARTESIAN_POINT('Ctrl Pts',(-18.8530026395886,1.75690876962598,0.));
#13203=CARTESIAN_POINT('Ctrl Pts',(-18.9002024267872,1.75429229572775,0.));
#13204=CARTESIAN_POINT('Ctrl Pts',(-18.947447637865,1.75080409924533,0.));
#13205=CARTESIAN_POINT('Ctrl Pts',(-18.9947239970259,1.74684309825012,0.));
#13206=CARTESIAN_POINT('Ctrl Pts',(-19.0420224296189,1.74256297552949,0.));
#13207=CARTESIAN_POINT('Ctrl Pts',(-19.0893375576541,1.73795301169841,0.));
#13208=CARTESIAN_POINT('Ctrl Pts',(-19.1366665585833,1.73290313712354,0.));
#13209=CARTESIAN_POINT('Ctrl Pts',(-19.1840079312107,1.72727220327098,0.));
#13210=CARTESIAN_POINT('Ctrl Pts',(-19.2313602042899,1.72096104670234,0.));
#13211=CARTESIAN_POINT('Ctrl Pts',(-19.2787209722437,1.71396454346262,0.));
#13212=CARTESIAN_POINT('Ctrl Pts',(-19.3260873558094,1.70633457265124,0.));
#13213=CARTESIAN_POINT('Ctrl Pts',(-19.3734562555057,1.69815571801252,0.));
#13214=CARTESIAN_POINT('Ctrl Pts',(-19.4208246682917,1.68951753233571,0.));
#13215=CARTESIAN_POINT('Ctrl Pts',(-19.4681900187091,1.68048476382294,0.));
#13216=CARTESIAN_POINT('Ctrl Pts',(-19.5155503513712,1.67107974760949,0.));
#13217=CARTESIAN_POINT('Ctrl Pts',(-19.5629041190868,1.66129908621006,0.));
#13218=CARTESIAN_POINT('Ctrl Pts',(-19.6102500448855,1.65112409599283,0.));
#13219=CARTESIAN_POINT('Ctrl Pts',(-19.6575869645839,1.64053294677822,0.));
#13220=CARTESIAN_POINT('Ctrl Pts',(-19.7049136553525,1.62951389038422,0.));
#13221=CARTESIAN_POINT('Ctrl Pts',(-19.7522287462982,1.61807191996834,0.));
#13222=CARTESIAN_POINT('Ctrl Pts',(-19.7995308006834,1.60622162219699,0.));
#13223=CARTESIAN_POINT('Ctrl Pts',(-19.8468183626037,1.59398289700559,0.));
#13224=CARTESIAN_POINT('Ctrl Pts',(-19.8940900137801,1.58137589158952,0.));
#13225=CARTESIAN_POINT('Ctrl Pts',(-19.9413444362352,1.56841542790453,0.));
#13226=CARTESIAN_POINT('Ctrl Pts',(-19.9885804375097,1.55510860515914,0.));
#13227=CARTESIAN_POINT('Ctrl Pts',(-20.0357969106526,1.54145790302918,0.));
#13228=CARTESIAN_POINT('Ctrl Pts',(-20.0829928089241,1.52746305716964,0.));
#13229=CARTESIAN_POINT('Ctrl Pts',(-20.1301671167606,1.51312326913583,0.));
#13230=CARTESIAN_POINT('Ctrl Pts',(-20.1773188177942,1.49843965844502,0.));
#13231=CARTESIAN_POINT('Ctrl Pts',(-20.224446881308,1.48341623961914,0.));
#13232=CARTESIAN_POINT('Ctrl Pts',(-20.2715502770004,1.46805861808021,0.));
#13233=CARTESIAN_POINT('Ctrl Pts',(-20.3186279833818,1.45237321894404,0.));
#13234=CARTESIAN_POINT('Ctrl Pts',(-20.3656789980171,1.43636637152782,0.));
#13235=CARTESIAN_POINT('Ctrl Pts',(-20.4127023494155,1.4200432946371,0.));
#13236=CARTESIAN_POINT('Ctrl Pts',(-20.4596971004275,1.40340771617025,0.));
#13237=CARTESIAN_POINT('Ctrl Pts',(-20.5066623390132,1.38646244026049,0.));
#13238=CARTESIAN_POINT('Ctrl Pts',(-20.5535971721246,1.36920969340018,0.));
#13239=CARTESIAN_POINT('Ctrl Pts',(-20.6005007190809,1.35165153211253,0.));
#13240=CARTESIAN_POINT('Ctrl Pts',(-20.6473721041685,1.33379029722591,0.));
#13241=CARTESIAN_POINT('Ctrl Pts',(-20.694210454218,1.31562879653596,0.));
#13242=CARTESIAN_POINT('Ctrl Pts',(-20.7410149035348,1.2971700649115,0.));
#13243=CARTESIAN_POINT('Ctrl Pts',(-20.7877845975367,1.27841722479262,0.));
#13244=CARTESIAN_POINT('Ctrl Pts',(-20.83451869657,1.25937332001005,0.));
#13245=CARTESIAN_POINT('Ctrl Pts',(-20.881216381382,1.24004113517905,0.));
#13246=CARTESIAN_POINT('Ctrl Pts',(-20.9278768531175,1.22042312071096,0.));
#13247=CARTESIAN_POINT('Ctrl Pts',(-20.9744993243732,1.20052150219503,0.));
#13248=CARTESIAN_POINT('Ctrl Pts',(-21.0210830121673,1.18033835060894,0.));
#13249=CARTESIAN_POINT('Ctrl Pts',(-21.0676271313238,1.15987566445807,0.));
#13250=CARTESIAN_POINT('Ctrl Pts',(-21.1141308858087,1.13913546246555,0.));
#13251=CARTESIAN_POINT('Ctrl Pts',(-21.1605934684164,1.11811982787747,0.));
#13252=CARTESIAN_POINT('Ctrl Pts',(-21.2070140764156,1.09683084929266,0.));
#13253=CARTESIAN_POINT('Ctrl Pts',(-21.2533919248553,1.07527058431887,0.));
#13254=CARTESIAN_POINT('Ctrl Pts',(-21.2997262593683,1.05344101900192,0.));
#13255=CARTESIAN_POINT('Ctrl Pts',(-21.3460163737343,1.03134402396953,0.));
#13256=CARTESIAN_POINT('Ctrl Pts',(-21.3922616124166,1.00898133629988,0.));
#13257=CARTESIAN_POINT('Ctrl Pts',(-21.4384613333266,0.986354611081137,
0.));
#13258=CARTESIAN_POINT('Ctrl Pts',(-21.4846148770804,0.963465462815773,
0.));
#13259=CARTESIAN_POINT('Ctrl Pts',(-21.5307215366685,0.940315509525154,
0.));
#13260=CARTESIAN_POINT('Ctrl Pts',(-21.5767805209408,0.916906425150856,
0.));
#13261=CARTESIAN_POINT('Ctrl Pts',(-21.6227909401433,0.893239967513676,
0.));
#13262=CARTESIAN_POINT('Ctrl Pts',(-21.6687518829182,0.869317897714101,
0.));
#13263=CARTESIAN_POINT('Ctrl Pts',(-21.7146624809285,0.845141916726562,
0.));
#13264=CARTESIAN_POINT('Ctrl Pts',(-21.7605219769118,0.82071359793408,0.));
#13265=CARTESIAN_POINT('Ctrl Pts',(-21.8063297959755,0.796034321106415,
0.));
#13266=CARTESIAN_POINT('Ctrl Pts',(-21.8612367655148,0.766119391688717,
0.));
#13267=CARTESIAN_POINT('Ctrl Pts',(-21.9069273598709,0.740879090965099,
0.));
#13268=CARTESIAN_POINT('Ctrl Pts',(-21.9434380560096,0.720488353007152,
0.));
#13269=CARTESIAN_POINT('Ctrl Pts',(-21.970797600548,0.705083756261763,0.));
#13270=CARTESIAN_POINT('Ctrl Pts',(-21.9890268624765,0.694764450219583,
0.));
#13271=CARTESIAN_POINT('Ctrl Pts',(-18.7118598491961,1.75362185428837,13.));
#13272=CARTESIAN_POINT('Ctrl Pts',(-18.7276767707249,1.75510417082366,13.));
#13273=CARTESIAN_POINT('Ctrl Pts',(-18.743509767289,1.75615601189424,13.));
#13274=CARTESIAN_POINT('Ctrl Pts',(-18.7593580381833,1.75680608702495,13.));
#13275=CARTESIAN_POINT('Ctrl Pts',(-18.77793339704,1.7575680237004,13.));
#13276=CARTESIAN_POINT('Ctrl Pts',(-18.796529725069,1.7577788791906,13.));
#13277=CARTESIAN_POINT('Ctrl Pts',(-18.8151436576367,1.75755628860693,13.));
#13278=CARTESIAN_POINT('Ctrl Pts',(-18.841334351583,1.75724309300298,13.));
#13279=CARTESIAN_POINT('Ctrl Pts',(-18.867559770113,1.75607893899574,13.));
#13280=CARTESIAN_POINT('Ctrl Pts',(-18.8938074357206,1.75447363677639,13.));
#13281=CARTESIAN_POINT('Ctrl Pts',(-18.9112662729044,1.75340585762614,13.));
#13282=CARTESIAN_POINT('Ctrl Pts',(-18.9287348768902,1.7521449293594,13.));
#13283=CARTESIAN_POINT('Ctrl Pts',(-18.9462100283356,1.75078122387574,13.));
#13284=CARTESIAN_POINT('Ctrl Pts',(-18.9646054898197,1.74934570031083,13.));
#13285=CARTESIAN_POINT('Ctrl Pts',(-18.9830081805109,1.74779717198811,13.));
#13286=CARTESIAN_POINT('Ctrl Pts',(-19.0014156957841,1.74617674699249,13.));
#13287=CARTESIAN_POINT('Ctrl Pts',(-19.0218582491316,1.74437717633198,13.));
#13288=CARTESIAN_POINT('Ctrl Pts',(-19.0423067706102,1.7424876259601,13.));
#13289=CARTESIAN_POINT('Ctrl Pts',(-19.0627595477341,1.74049525500348,13.));
#13290=CARTESIAN_POINT('Ctrl Pts',(-19.0935931019431,1.73749165908478,13.));
#13291=CARTESIAN_POINT('Ctrl Pts',(-19.124436353955,1.73424805120453,13.));
#13292=CARTESIAN_POINT('Ctrl Pts',(-19.155287003777,1.73060838684868,13.));
#13293=CARTESIAN_POINT('Ctrl Pts',(-19.1776993264081,1.72796425026539,13.));
#13294=CARTESIAN_POINT('Ctrl Pts',(-19.2001156538104,1.72510779282378,13.));
#13295=CARTESIAN_POINT('Ctrl Pts',(-19.2225350169938,1.72201836571105,13.));
#13296=CARTESIAN_POINT('Ctrl Pts',(-19.2499407687534,1.71824180560815,13.));
#13297=CARTESIAN_POINT('Ctrl Pts',(-19.2773510352597,1.71411839343645,13.));
#13298=CARTESIAN_POINT('Ctrl Pts',(-19.3047632983727,1.70969587297193,13.));
#13299=CARTESIAN_POINT('Ctrl Pts',(-19.3343730920364,1.70491881688253,13.));
#13300=CARTESIAN_POINT('Ctrl Pts',(-19.3639851445252,1.69979875336516,13.));
#13301=CARTESIAN_POINT('Ctrl Pts',(-19.3935962281375,1.69442732753347,13.));
#13302=CARTESIAN_POINT('Ctrl Pts',(-19.4209330414363,1.68946845243685,13.));
#13303=CARTESIAN_POINT('Ctrl Pts',(-19.448269005347,1.68429785630172,13.));
#13304=CARTESIAN_POINT('Ctrl Pts',(-19.4756022976243,1.67894398811971,13.));
#13305=CARTESIAN_POINT('Ctrl Pts',(-19.5127359786207,1.67167048329817,13.));
#13306=CARTESIAN_POINT('Ctrl Pts',(-19.5498647402244,1.66405675112121,13.));
#13307=CARTESIAN_POINT('Ctrl Pts',(-19.5869856493979,1.65607285222827,13.));
#13308=CARTESIAN_POINT('Ctrl Pts',(-19.6228065250069,1.64836856223413,13.));
#13309=CARTESIAN_POINT('Ctrl Pts',(-19.6586201923617,1.64031177032422,13.));
#13310=CARTESIAN_POINT('Ctrl Pts',(-19.6944241981293,1.63188637918844,13.));
#13311=CARTESIAN_POINT('Ctrl Pts',(-19.7430649431878,1.62044024925217,13.));
#13312=CARTESIAN_POINT('Ctrl Pts',(-19.7916877990604,1.60831707818014,13.));
#13313=CARTESIAN_POINT('Ctrl Pts',(-19.8402857466125,1.59560243913608,13.));
#13314=CARTESIAN_POINT('Ctrl Pts',(-19.8830022860036,1.58442654782939,13.));
#13315=CARTESIAN_POINT('Ctrl Pts',(-19.9256995150218,1.5728005280582,13.));
#13316=CARTESIAN_POINT('Ctrl Pts',(-19.9683733417696,1.56075644050925,13.));
#13317=CARTESIAN_POINT('Ctrl Pts',(-20.0312849226892,1.54300053141499,13.));
#13318=CARTESIAN_POINT('Ctrl Pts',(-20.0941457150012,1.52432694533036,13.));
#13319=CARTESIAN_POINT('Ctrl Pts',(-20.1569447710111,1.50474000384183,13.));
#13320=CARTESIAN_POINT('Ctrl Pts',(-20.236197792604,1.48002109251801,13.));
#13321=CARTESIAN_POINT('Ctrl Pts',(-20.3153523889882,1.45385270862993,13.));
#13322=CARTESIAN_POINT('Ctrl Pts',(-20.3943871107868,1.42635858933979,13.));
#13323=CARTESIAN_POINT('Ctrl Pts',(-20.501445734804,1.3891156850468,13.));
#13324=CARTESIAN_POINT('Ctrl Pts',(-20.6082844519781,1.34943433503116,13.));
#13325=CARTESIAN_POINT('Ctrl Pts',(-20.7148563913884,1.30744723530953,13.));
#13326=CARTESIAN_POINT('Ctrl Pts',(-20.8098680661395,1.27001463640438,13.));
#13327=CARTESIAN_POINT('Ctrl Pts',(-20.9046675819257,1.23075788115688,13.));
#13328=CARTESIAN_POINT('Ctrl Pts',(-20.9992246138437,1.18977154285938,13.));
#13329=CARTESIAN_POINT('Ctrl Pts',(-21.1332379309096,1.13168263039858,13.));
#13330=CARTESIAN_POINT('Ctrl Pts',(-21.2667633190703,1.07011397729315,13.));
#13331=CARTESIAN_POINT('Ctrl Pts',(-21.399720077537,1.00527632074311,13.));
#13332=CARTESIAN_POINT('Ctrl Pts',(-21.5029977299653,0.954911968944342,
13.));
#13333=CARTESIAN_POINT('Ctrl Pts',(-21.6059349891428,0.902570955669054,
13.));
#13334=CARTESIAN_POINT('Ctrl Pts',(-21.7084903368843,0.848338494786424,
13.));
#13335=CARTESIAN_POINT('Ctrl Pts',(-21.7972084624612,0.801423317948843,
13.));
#13336=CARTESIAN_POINT('Ctrl Pts',(-21.8856382926503,0.753096148034919,
13.));
#13337=CARTESIAN_POINT('Ctrl Pts',(-21.9737740854159,0.703383282495547,
13.));
#13338=CARTESIAN_POINT('Ctrl Pts',(-21.9788593181079,0.700514964402279,
13.));
#13339=CARTESIAN_POINT('Ctrl Pts',(-21.983943577112,0.697642020224148,13.));
#13340=CARTESIAN_POINT('Ctrl Pts',(-21.9890268624765,0.694764450219584,
13.));
#13341=CARTESIAN_POINT('Ctrl Pts',(-21.1275013067528,6.1342227326009,0.));
#13342=CARTESIAN_POINT('Ctrl Pts',(-21.1275013067528,6.1342227326009,21.));
#13343=CARTESIAN_POINT('Ctrl Pts',(-21.1204271980506,6.12649903511517,0.));
#13344=CARTESIAN_POINT('Ctrl Pts',(-21.1204271980506,6.12649903511517,21.));
#13345=CARTESIAN_POINT('Ctrl Pts',(-21.1062663590356,6.11107360216958,0.));
#13346=CARTESIAN_POINT('Ctrl Pts',(-21.1062663590356,6.11107360216958,21.));
#13347=CARTESIAN_POINT('Ctrl Pts',(-21.0849872356853,6.08800133883114,0.));
#13348=CARTESIAN_POINT('Ctrl Pts',(-21.0849872356853,6.08800133883114,21.));
#13349=CARTESIAN_POINT('Ctrl Pts',(-21.0565393163693,6.05737013696533,0.));
#13350=CARTESIAN_POINT('Ctrl Pts',(-21.0565393163693,6.05737013696533,21.));
#13351=CARTESIAN_POINT('Ctrl Pts',(-21.0208530236003,6.01930117633045,0.));
#13352=CARTESIAN_POINT('Ctrl Pts',(-21.0208530236003,6.01930117633045,21.));
#13353=CARTESIAN_POINT('Ctrl Pts',(-20.9850401822713,5.98145286361837,0.));
#13354=CARTESIAN_POINT('Ctrl Pts',(-20.9850401822713,5.98145286361837,21.));
#13355=CARTESIAN_POINT('Ctrl Pts',(-20.9491006734021,5.94382608200804,0.));
#13356=CARTESIAN_POINT('Ctrl Pts',(-20.9491006734021,5.94382608200804,21.));
#13357=CARTESIAN_POINT('Ctrl Pts',(-20.9130344665641,5.906422006626,0.));
#13358=CARTESIAN_POINT('Ctrl Pts',(-20.9130344665641,5.906422006626,21.));
#13359=CARTESIAN_POINT('Ctrl Pts',(-20.8768416821402,5.86924212736288,0.));
#13360=CARTESIAN_POINT('Ctrl Pts',(-20.8768416821402,5.86924212736288,21.));
#13361=CARTESIAN_POINT('Ctrl Pts',(-20.8405225541277,5.83228817460178,0.));
#13362=CARTESIAN_POINT('Ctrl Pts',(-20.8405225541277,5.83228817460178,21.));
#13363=CARTESIAN_POINT('Ctrl Pts',(-20.8040773827343,5.79556203439644,0.));
#13364=CARTESIAN_POINT('Ctrl Pts',(-20.8040773827343,5.79556203439644,21.));
#13365=CARTESIAN_POINT('Ctrl Pts',(-20.7675064905026,5.75906566327796,0.));
#13366=CARTESIAN_POINT('Ctrl Pts',(-20.7675064905026,5.75906566327796,21.));
#13367=CARTESIAN_POINT('Ctrl Pts',(-20.7308101804425,5.72280100798241,0.));
#13368=CARTESIAN_POINT('Ctrl Pts',(-20.7308101804425,5.72280100798241,21.));
#13369=CARTESIAN_POINT('Ctrl Pts',(-20.6939886877061,5.68676990500163,0.));
#13370=CARTESIAN_POINT('Ctrl Pts',(-20.6939886877061,5.68676990500163,21.));
#13371=CARTESIAN_POINT('Ctrl Pts',(-20.6570421847033,5.65097411164335,0.));
#13372=CARTESIAN_POINT('Ctrl Pts',(-20.6570421847033,5.65097411164335,21.));
#13373=CARTESIAN_POINT('Ctrl Pts',(-20.6199707996366,5.61541536715149,0.));
#13374=CARTESIAN_POINT('Ctrl Pts',(-20.6199707996366,5.61541536715149,21.));
#13375=CARTESIAN_POINT('Ctrl Pts',(-20.5827746317185,5.58009544402475,0.));
#13376=CARTESIAN_POINT('Ctrl Pts',(-20.5827746317185,5.58009544402475,21.));
#13377=CARTESIAN_POINT('Ctrl Pts',(-20.5454537676144,5.5450161968946,0.));
#13378=CARTESIAN_POINT('Ctrl Pts',(-20.5454537676144,5.5450161968946,21.));
#13379=CARTESIAN_POINT('Ctrl Pts',(-20.5080083009242,5.51017962306782,0.));
#13380=CARTESIAN_POINT('Ctrl Pts',(-20.5080083009242,5.51017962306782,21.));
#13381=CARTESIAN_POINT('Ctrl Pts',(-20.4704383353718,5.47558784449851,0.));
#13382=CARTESIAN_POINT('Ctrl Pts',(-20.4704383353718,5.47558784449851,21.));
#13383=CARTESIAN_POINT('Ctrl Pts',(-20.4327439816542,5.44124306065111,0.));
#13384=CARTESIAN_POINT('Ctrl Pts',(-20.4327439816542,5.44124306065111,21.));
#13385=CARTESIAN_POINT('Ctrl Pts',(-20.3949253578015,5.40714750595875,0.));
#13386=CARTESIAN_POINT('Ctrl Pts',(-20.3949253578015,5.40714750595875,21.));
#13387=CARTESIAN_POINT('Ctrl Pts',(-20.3569825877537,5.37330341114649,0.));
#13388=CARTESIAN_POINT('Ctrl Pts',(-20.3569825877537,5.37330341114649,21.));
#13389=CARTESIAN_POINT('Ctrl Pts',(-20.3189158047642,5.33971294212214,0.));
#13390=CARTESIAN_POINT('Ctrl Pts',(-20.3189158047642,5.33971294212214,21.));
#13391=CARTESIAN_POINT('Ctrl Pts',(-20.2807251380077,5.30637824220997,0.));
#13392=CARTESIAN_POINT('Ctrl Pts',(-20.2807251380077,5.30637824220997,21.));
#13393=CARTESIAN_POINT('Ctrl Pts',(-20.2424106921768,5.2733015229815,0.));
#13394=CARTESIAN_POINT('Ctrl Pts',(-20.2424106921768,5.2733015229815,21.));
#13395=CARTESIAN_POINT('Ctrl Pts',(-20.2039725283917,5.2404851444189,0.));
#13396=CARTESIAN_POINT('Ctrl Pts',(-20.2039725283917,5.2404851444189,21.));
#13397=CARTESIAN_POINT('Ctrl Pts',(-20.1654106491899,5.20793168386163,0.));
#13398=CARTESIAN_POINT('Ctrl Pts',(-20.1654106491899,5.20793168386163,21.));
#13399=CARTESIAN_POINT('Ctrl Pts',(-20.1267249732337,5.17564404279922,0.));
#13400=CARTESIAN_POINT('Ctrl Pts',(-20.1267249732337,5.17564404279922,21.));
#13401=CARTESIAN_POINT('Ctrl Pts',(-20.087915358486,5.14362537555398,0.));
#13402=CARTESIAN_POINT('Ctrl Pts',(-20.087915358486,5.14362537555398,21.));
#13403=CARTESIAN_POINT('Ctrl Pts',(-20.0489816528155,5.11187891582335,0.));
#13404=CARTESIAN_POINT('Ctrl Pts',(-20.0489816528155,5.11187891582335,21.));
#13405=CARTESIAN_POINT('Ctrl Pts',(-20.0099237417205,5.08040781745336,0.));
#13406=CARTESIAN_POINT('Ctrl Pts',(-20.0099237417205,5.08040781745336,21.));
#13407=CARTESIAN_POINT('Ctrl Pts',(-19.9707415879783,5.04921502064063,0.));
#13408=CARTESIAN_POINT('Ctrl Pts',(-19.9707415879783,5.04921502064063,21.));
#13409=CARTESIAN_POINT('Ctrl Pts',(-19.931435301086,5.01830302225557,0.));
#13410=CARTESIAN_POINT('Ctrl Pts',(-19.931435301086,5.01830302225557,21.));
#13411=CARTESIAN_POINT('Ctrl Pts',(-19.8920050831202,4.98767405031333,0.));
#13412=CARTESIAN_POINT('Ctrl Pts',(-19.8920050831202,4.98767405031333,21.));
#13413=CARTESIAN_POINT('Ctrl Pts',(-19.8524510953961,4.95733049830096,0.));
#13414=CARTESIAN_POINT('Ctrl Pts',(-19.8524510953961,4.95733049830096,21.));
#13415=CARTESIAN_POINT('Ctrl Pts',(-19.8127733387903,4.92727531494347,0.));
#13416=CARTESIAN_POINT('Ctrl Pts',(-19.8127733387903,4.92727531494347,21.));
#13417=CARTESIAN_POINT('Ctrl Pts',(-19.772971552601,4.89751233527804,0.));
#13418=CARTESIAN_POINT('Ctrl Pts',(-19.772971552601,4.89751233527804,21.));
#13419=CARTESIAN_POINT('Ctrl Pts',(-19.7330450480715,4.86804682289087,0.));
#13420=CARTESIAN_POINT('Ctrl Pts',(-19.7330450480715,4.86804682289087,21.));
#13421=CARTESIAN_POINT('Ctrl Pts',(-19.6929928227072,4.83888510708974,0.));
#13422=CARTESIAN_POINT('Ctrl Pts',(-19.6929928227072,4.83888510708974,21.));
#13423=CARTESIAN_POINT('Ctrl Pts',(-19.6528138625329,4.81003361418061,0.));
#13424=CARTESIAN_POINT('Ctrl Pts',(-19.6528138625329,4.81003361418061,21.));
#13425=CARTESIAN_POINT('Ctrl Pts',(-19.6125074152527,4.7814979936173,0.));
#13426=CARTESIAN_POINT('Ctrl Pts',(-19.6125074152527,4.7814979936173,21.));
#13427=CARTESIAN_POINT('Ctrl Pts',(-19.5720732205813,4.75328238194611,0.));
#13428=CARTESIAN_POINT('Ctrl Pts',(-19.5720732205813,4.75328238194611,21.));
#13429=CARTESIAN_POINT('Ctrl Pts',(-19.531511899192,4.72538815796615,0.));
#13430=CARTESIAN_POINT('Ctrl Pts',(-19.531511899192,4.72538815796615,21.));
#13431=CARTESIAN_POINT('Ctrl Pts',(-19.4908246636763,4.69781487613784,0.));
#13432=CARTESIAN_POINT('Ctrl Pts',(-19.4908246636763,4.69781487613784,21.));
#13433=CARTESIAN_POINT('Ctrl Pts',(-19.4500125912299,4.67056260851453,0.));
#13434=CARTESIAN_POINT('Ctrl Pts',(-19.4500125912299,4.67056260851453,21.));
#13435=CARTESIAN_POINT('Ctrl Pts',(-19.4090759683639,4.64363405547472,0.));
#13436=CARTESIAN_POINT('Ctrl Pts',(-19.4090759683639,4.64363405547472,21.));
#13437=CARTESIAN_POINT('Ctrl Pts',(-19.3680137353983,4.61703633725712,0.));
#13438=CARTESIAN_POINT('Ctrl Pts',(-19.3680137353983,4.61703633725712,21.));
#13439=CARTESIAN_POINT('Ctrl Pts',(-19.3268225655679,4.59078395765677,0.));
#13440=CARTESIAN_POINT('Ctrl Pts',(-19.3268225655679,4.59078395765677,21.));
#13441=CARTESIAN_POINT('Ctrl Pts',(-19.2854975819105,4.56489651606741,0.));
#13442=CARTESIAN_POINT('Ctrl Pts',(-19.2854975819105,4.56489651606741,21.));
#13443=CARTESIAN_POINT('Ctrl Pts',(-19.2440340196551,4.53939338835152,0.));
#13444=CARTESIAN_POINT('Ctrl Pts',(-19.2440340196551,4.53939338835152,21.));
#13445=CARTESIAN_POINT('Ctrl Pts',(-19.2024287376926,4.51428889122955,0.));
#13446=CARTESIAN_POINT('Ctrl Pts',(-19.2024287376926,4.51428889122955,21.));
#13447=CARTESIAN_POINT('Ctrl Pts',(-19.1606814968494,4.48958819710577,0.));
#13448=CARTESIAN_POINT('Ctrl Pts',(-19.1606814968494,4.48958819710577,21.));
#13449=CARTESIAN_POINT('Ctrl Pts',(-19.1187970904933,4.46528051067021,0.));
#13450=CARTESIAN_POINT('Ctrl Pts',(-19.1187970904933,4.46528051067021,21.));
#13451=CARTESIAN_POINT('Ctrl Pts',(-19.0767833717249,4.44134542994082,0.));
#13452=CARTESIAN_POINT('Ctrl Pts',(-19.0767833717249,4.44134542994082,21.));
#13453=CARTESIAN_POINT('Ctrl Pts',(-19.034647328575,4.41776558033332,0.));
#13454=CARTESIAN_POINT('Ctrl Pts',(-19.034647328575,4.41776558033332,21.));
#13455=CARTESIAN_POINT('Ctrl Pts',(-18.9923914823906,4.39453820875555,0.));
#13456=CARTESIAN_POINT('Ctrl Pts',(-18.9923914823906,4.39453820875555,21.));
#13457=CARTESIAN_POINT('Ctrl Pts',(-18.9500107909187,4.37168516143122,0.));
#13458=CARTESIAN_POINT('Ctrl Pts',(-18.9500107909187,4.37168516143122,21.));
#13459=CARTESIAN_POINT('Ctrl Pts',(-18.9074876952706,4.34926881342022,0.));
#13460=CARTESIAN_POINT('Ctrl Pts',(-18.9074876952706,4.34926881342022,21.));
#13461=CARTESIAN_POINT('Ctrl Pts',(-18.8647973781745,4.32737526247704,0.));
#13462=CARTESIAN_POINT('Ctrl Pts',(-18.8647973781745,4.32737526247704,21.));
#13463=CARTESIAN_POINT('Ctrl Pts',(-18.8219166495975,4.30608591031526,0.));
#13464=CARTESIAN_POINT('Ctrl Pts',(-18.8219166495975,4.30608591031526,21.));
#13465=CARTESIAN_POINT('Ctrl Pts',(-18.778832216358,4.28545098663153,0.));
#13466=CARTESIAN_POINT('Ctrl Pts',(-18.778832216358,4.28545098663153,21.));
#13467=CARTESIAN_POINT('Ctrl Pts',(-18.735547949685,4.26546636161933,0.));
#13468=CARTESIAN_POINT('Ctrl Pts',(-18.735547949685,4.26546636161933,21.));
#13469=CARTESIAN_POINT('Ctrl Pts',(-18.6920958920047,4.24603817988452,0.));
#13470=CARTESIAN_POINT('Ctrl Pts',(-18.6920958920047,4.24603817988452,21.));
#13471=CARTESIAN_POINT('Ctrl Pts',(-18.6485210883348,4.22703266508919,0.));
#13472=CARTESIAN_POINT('Ctrl Pts',(-18.6485210883348,4.22703266508919,21.));
#13473=CARTESIAN_POINT('Ctrl Pts',(-18.6048602364653,4.20834600700665,0.));
#13474=CARTESIAN_POINT('Ctrl Pts',(-18.6048602364653,4.20834600700665,21.));
#13475=CARTESIAN_POINT('Ctrl Pts',(-18.5611217636409,4.18996967278621,0.));
#13476=CARTESIAN_POINT('Ctrl Pts',(-18.5611217636409,4.18996967278621,21.));
#13477=CARTESIAN_POINT('Ctrl Pts',(-18.5172668097744,4.17205262766562,0.));
#13478=CARTESIAN_POINT('Ctrl Pts',(-18.5172668097744,4.17205262766562,21.));
#13479=CARTESIAN_POINT('Ctrl Pts',(-18.4731856794913,4.15497867673974,0.));
#13480=CARTESIAN_POINT('Ctrl Pts',(-18.4731856794913,4.15497867673974,21.));
#13481=CARTESIAN_POINT('Ctrl Pts',(-18.4287286547442,4.13926275457062,0.));
#13482=CARTESIAN_POINT('Ctrl Pts',(-18.4287286547442,4.13926275457062,21.));
#13483=CARTESIAN_POINT('Ctrl Pts',(-18.3927403741815,4.12819301671079,0.));
#13484=CARTESIAN_POINT('Ctrl Pts',(-18.3927403741815,4.12819301671079,21.));
#13485=CARTESIAN_POINT('Ctrl Pts',(-18.3654573320481,4.1209201986886,0.));
#13486=CARTESIAN_POINT('Ctrl Pts',(-18.3654573320481,4.1209201986886,21.));
#13487=CARTESIAN_POINT('Ctrl Pts',(-18.3471320125699,4.11655269114951,0.));
#13488=CARTESIAN_POINT('Ctrl Pts',(-18.3471320125699,4.11655269114951,21.));
#13489=CARTESIAN_POINT('Ctrl Pts',(-18.337935196262,4.11448919812531,0.));
#13490=CARTESIAN_POINT('Ctrl Pts',(-18.337935196262,4.11448919812531,21.));
#13491=CARTESIAN_POINT('',(-21.1275013067528,6.13422273260085,0.));
#13492=CARTESIAN_POINT('Ctrl Pts',(-18.337935196262,4.11448919812531,0.));
#13493=CARTESIAN_POINT('Ctrl Pts',(-18.3471320125699,4.11655269114951,0.));
#13494=CARTESIAN_POINT('Ctrl Pts',(-18.3654573320481,4.1209201986886,0.));
#13495=CARTESIAN_POINT('Ctrl Pts',(-18.3927403741815,4.12819301671079,0.));
#13496=CARTESIAN_POINT('Ctrl Pts',(-18.4287286547442,4.13926275457062,0.));
#13497=CARTESIAN_POINT('Ctrl Pts',(-18.4731856794913,4.15497867673974,0.));
#13498=CARTESIAN_POINT('Ctrl Pts',(-18.5172668097744,4.17205262766562,0.));
#13499=CARTESIAN_POINT('Ctrl Pts',(-18.5611217636409,4.18996967278621,0.));
#13500=CARTESIAN_POINT('Ctrl Pts',(-18.6048602364653,4.20834600700665,0.));
#13501=CARTESIAN_POINT('Ctrl Pts',(-18.6485210883348,4.22703266508919,0.));
#13502=CARTESIAN_POINT('Ctrl Pts',(-18.6920958920047,4.24603817988452,0.));
#13503=CARTESIAN_POINT('Ctrl Pts',(-18.735547949685,4.26546636161933,0.));
#13504=CARTESIAN_POINT('Ctrl Pts',(-18.778832216358,4.28545098663153,0.));
#13505=CARTESIAN_POINT('Ctrl Pts',(-18.8219166495975,4.30608591031526,0.));
#13506=CARTESIAN_POINT('Ctrl Pts',(-18.8647973781745,4.32737526247704,0.));
#13507=CARTESIAN_POINT('Ctrl Pts',(-18.9074876952706,4.34926881342022,0.));
#13508=CARTESIAN_POINT('Ctrl Pts',(-18.9500107909187,4.37168516143122,0.));
#13509=CARTESIAN_POINT('Ctrl Pts',(-18.9923914823906,4.39453820875555,0.));
#13510=CARTESIAN_POINT('Ctrl Pts',(-19.034647328575,4.41776558033332,0.));
#13511=CARTESIAN_POINT('Ctrl Pts',(-19.0767833717249,4.44134542994082,0.));
#13512=CARTESIAN_POINT('Ctrl Pts',(-19.1187970904933,4.46528051067021,0.));
#13513=CARTESIAN_POINT('Ctrl Pts',(-19.1606814968494,4.48958819710577,0.));
#13514=CARTESIAN_POINT('Ctrl Pts',(-19.2024287376926,4.51428889122955,0.));
#13515=CARTESIAN_POINT('Ctrl Pts',(-19.2440340196551,4.53939338835152,0.));
#13516=CARTESIAN_POINT('Ctrl Pts',(-19.2854975819105,4.56489651606741,0.));
#13517=CARTESIAN_POINT('Ctrl Pts',(-19.3268225655679,4.59078395765677,0.));
#13518=CARTESIAN_POINT('Ctrl Pts',(-19.3680137353983,4.61703633725712,0.));
#13519=CARTESIAN_POINT('Ctrl Pts',(-19.4090759683639,4.64363405547472,0.));
#13520=CARTESIAN_POINT('Ctrl Pts',(-19.4500125912299,4.67056260851453,0.));
#13521=CARTESIAN_POINT('Ctrl Pts',(-19.4908246636763,4.69781487613784,0.));
#13522=CARTESIAN_POINT('Ctrl Pts',(-19.531511899192,4.72538815796615,0.));
#13523=CARTESIAN_POINT('Ctrl Pts',(-19.5720732205813,4.75328238194611,0.));
#13524=CARTESIAN_POINT('Ctrl Pts',(-19.6125074152527,4.7814979936173,0.));
#13525=CARTESIAN_POINT('Ctrl Pts',(-19.6528138625329,4.81003361418061,0.));
#13526=CARTESIAN_POINT('Ctrl Pts',(-19.6929928227072,4.83888510708974,0.));
#13527=CARTESIAN_POINT('Ctrl Pts',(-19.7330450480715,4.86804682289087,0.));
#13528=CARTESIAN_POINT('Ctrl Pts',(-19.772971552601,4.89751233527804,0.));
#13529=CARTESIAN_POINT('Ctrl Pts',(-19.8127733387903,4.92727531494347,0.));
#13530=CARTESIAN_POINT('Ctrl Pts',(-19.8524510953961,4.95733049830096,0.));
#13531=CARTESIAN_POINT('Ctrl Pts',(-19.8920050831202,4.98767405031333,0.));
#13532=CARTESIAN_POINT('Ctrl Pts',(-19.931435301086,5.01830302225557,0.));
#13533=CARTESIAN_POINT('Ctrl Pts',(-19.9707415879783,5.04921502064063,0.));
#13534=CARTESIAN_POINT('Ctrl Pts',(-20.0099237417205,5.08040781745336,0.));
#13535=CARTESIAN_POINT('Ctrl Pts',(-20.0489816528155,5.11187891582335,0.));
#13536=CARTESIAN_POINT('Ctrl Pts',(-20.087915358486,5.14362537555398,0.));
#13537=CARTESIAN_POINT('Ctrl Pts',(-20.1267249732337,5.17564404279922,0.));
#13538=CARTESIAN_POINT('Ctrl Pts',(-20.1654106491899,5.20793168386163,0.));
#13539=CARTESIAN_POINT('Ctrl Pts',(-20.2039725283917,5.2404851444189,0.));
#13540=CARTESIAN_POINT('Ctrl Pts',(-20.2424106921768,5.2733015229815,0.));
#13541=CARTESIAN_POINT('Ctrl Pts',(-20.2807251380077,5.30637824220997,0.));
#13542=CARTESIAN_POINT('Ctrl Pts',(-20.3189158047642,5.33971294212214,0.));
#13543=CARTESIAN_POINT('Ctrl Pts',(-20.3569825877537,5.37330341114649,0.));
#13544=CARTESIAN_POINT('Ctrl Pts',(-20.3949253578015,5.40714750595875,0.));
#13545=CARTESIAN_POINT('Ctrl Pts',(-20.4327439816542,5.44124306065111,0.));
#13546=CARTESIAN_POINT('Ctrl Pts',(-20.4704383353718,5.47558784449851,0.));
#13547=CARTESIAN_POINT('Ctrl Pts',(-20.5080083009242,5.51017962306782,0.));
#13548=CARTESIAN_POINT('Ctrl Pts',(-20.5454537676144,5.5450161968946,0.));
#13549=CARTESIAN_POINT('Ctrl Pts',(-20.5827746317185,5.58009544402475,0.));
#13550=CARTESIAN_POINT('Ctrl Pts',(-20.6199707996366,5.61541536715149,0.));
#13551=CARTESIAN_POINT('Ctrl Pts',(-20.6570421847033,5.65097411164335,0.));
#13552=CARTESIAN_POINT('Ctrl Pts',(-20.6939886877061,5.68676990500163,0.));
#13553=CARTESIAN_POINT('Ctrl Pts',(-20.7308101804425,5.72280100798241,0.));
#13554=CARTESIAN_POINT('Ctrl Pts',(-20.7675064905026,5.75906566327796,0.));
#13555=CARTESIAN_POINT('Ctrl Pts',(-20.8040773827343,5.79556203439644,0.));
#13556=CARTESIAN_POINT('Ctrl Pts',(-20.8405225541277,5.83228817460178,0.));
#13557=CARTESIAN_POINT('Ctrl Pts',(-20.8768416821402,5.86924212736288,0.));
#13558=CARTESIAN_POINT('Ctrl Pts',(-20.9130344665641,5.906422006626,0.));
#13559=CARTESIAN_POINT('Ctrl Pts',(-20.9491006734021,5.94382608200804,0.));
#13560=CARTESIAN_POINT('Ctrl Pts',(-20.9850401822713,5.98145286361837,0.));
#13561=CARTESIAN_POINT('Ctrl Pts',(-21.0280155918661,6.02687083887287,0.));
#13562=CARTESIAN_POINT('Ctrl Pts',(-21.0636702474951,6.06499496148845,0.));
#13563=CARTESIAN_POINT('Ctrl Pts',(-21.0920928984154,6.09567013127871,0.));
#13564=CARTESIAN_POINT('Ctrl Pts',(-21.1133530893457,6.11877533761502,0.));
#13565=CARTESIAN_POINT('Ctrl Pts',(-21.1275013067528,6.1342227326009,0.));
#13566=CARTESIAN_POINT('',(-21.1275013067528,6.13422273260085,13.));
#13567=CARTESIAN_POINT('Ctrl Pts',(-21.1275013067528,6.1342227326009,13.));
#13568=CARTESIAN_POINT('Ctrl Pts',(-21.0578559230999,6.05818207543008,13.));
#13569=CARTESIAN_POINT('Ctrl Pts',(-20.9874765053145,5.98341417321284,13.));
#13570=CARTESIAN_POINT('Ctrl Pts',(-20.9163599174182,5.90994468906837,13.));
#13571=CARTESIAN_POINT('Ctrl Pts',(-20.7985166493983,5.78820257000103,13.));
#13572=CARTESIAN_POINT('Ctrl Pts',(-20.6786545111106,5.6700381210249,13.));
#13573=CARTESIAN_POINT('Ctrl Pts',(-20.5568063022896,5.55573864053401,13.));
#13574=CARTESIAN_POINT('Ctrl Pts',(-20.4631466243016,5.46788135776747,13.));
#13575=CARTESIAN_POINT('Ctrl Pts',(-20.3683108787545,5.38230707413678,13.));
#13576=CARTESIAN_POINT('Ctrl Pts',(-20.2723075600433,5.29917141679073,13.));
#13577=CARTESIAN_POINT('Ctrl Pts',(-20.1689623028903,5.20967788675077,13.));
#13578=CARTESIAN_POINT('Ctrl Pts',(-20.0642651129984,5.12300396079329,13.));
#13579=CARTESIAN_POINT('Ctrl Pts',(-19.9582092070171,5.03941267576854,13.));
#13580=CARTESIAN_POINT('Ctrl Pts',(-19.8994937738184,4.99313426754168,13.));
#13581=CARTESIAN_POINT('Ctrl Pts',(-19.8403635608621,4.94779583996753,13.));
#13582=CARTESIAN_POINT('Ctrl Pts',(-19.7808173213525,4.90344584505529,13.));
#13583=CARTESIAN_POINT('Ctrl Pts',(-19.7234362340388,4.86070845388874,13.));
#13584=CARTESIAN_POINT('Ctrl Pts',(-19.665666793332,4.8188953867059,13.));
#13585=CARTESIAN_POINT('Ctrl Pts',(-19.6074986353569,4.77808296524689,13.));
#13586=CARTESIAN_POINT('Ctrl Pts',(-19.5572235046905,4.74280851453208,13.));
#13587=CARTESIAN_POINT('Ctrl Pts',(-19.5066514987622,4.70827845283243,13.));
#13588=CARTESIAN_POINT('Ctrl Pts',(-19.4557905169783,4.67449772127139,13.));
#13589=CARTESIAN_POINT('Ctrl Pts',(-19.4192898917399,4.65025481876063,13.));
#13590=CARTESIAN_POINT('Ctrl Pts',(-19.382641288418,4.62639514817842,13.));
#13591=CARTESIAN_POINT('Ctrl Pts',(-19.3458364380218,4.60295743043302,13.));
#13592=CARTESIAN_POINT('Ctrl Pts',(-19.3096309080951,4.57990136629721,13.));
#13593=CARTESIAN_POINT('Ctrl Pts',(-19.2732722733459,4.55725971973435,13.));
#13594=CARTESIAN_POINT('Ctrl Pts',(-19.2367485574674,4.53508357551694,13.));
#13595=CARTESIAN_POINT('Ctrl Pts',(-19.205080350215,4.51585555574276,13.));
#13596=CARTESIAN_POINT('Ctrl Pts',(-19.1732873011956,4.49697986249447,13.));
#13597=CARTESIAN_POINT('Ctrl Pts',(-19.1413765620497,4.47844262259009,13.));
#13598=CARTESIAN_POINT('Ctrl Pts',(-19.1124727543428,4.4616521366297,13.));
#13599=CARTESIAN_POINT('Ctrl Pts',(-19.083474045539,4.44513401120468,13.));
#13600=CARTESIAN_POINT('Ctrl Pts',(-19.0543895551234,4.42886646462772,13.));
#13601=CARTESIAN_POINT('Ctrl Pts',(-19.0298903165561,4.41516354259612,13.));
#13602=CARTESIAN_POINT('Ctrl Pts',(-19.0053307305268,4.40163676081042,13.));
#13603=CARTESIAN_POINT('Ctrl Pts',(-18.9807063063319,4.38830551702962,13.));
#13604=CARTESIAN_POINT('Ctrl Pts',(-18.9450720846902,4.36901375646356,13.));
#13605=CARTESIAN_POINT('Ctrl Pts',(-18.9093017976668,4.35013223004763,13.));
#13606=CARTESIAN_POINT('Ctrl Pts',(-18.8733353265524,4.33187128675496,13.));
#13607=CARTESIAN_POINT('Ctrl Pts',(-18.8516029898089,4.32083731659903,13.));
#13608=CARTESIAN_POINT('Ctrl Pts',(-18.8297980042953,4.31003325590031,13.));
#13609=CARTESIAN_POINT('Ctrl Pts',(-18.8079138030273,4.29948469308613,13.));
#13610=CARTESIAN_POINT('Ctrl Pts',(-18.7877304129875,4.28975595064628,13.));
#13611=CARTESIAN_POINT('Ctrl Pts',(-18.7674792482884,4.28024580006689,13.));
#13612=CARTESIAN_POINT('Ctrl Pts',(-18.7471689058935,4.27093067982675,13.));
#13613=CARTESIAN_POINT('Ctrl Pts',(-18.7192299720641,4.25811678811867,13.));
#13614=CARTESIAN_POINT('Ctrl Pts',(-18.6911811213665,4.24566493398838,13.));
#13615=CARTESIAN_POINT('Ctrl Pts',(-18.663071173524,4.23343245340777,13.));
#13616=CARTESIAN_POINT('Ctrl Pts',(-18.6452377209097,4.2256719494036,13.));
#13617=CARTESIAN_POINT('Ctrl Pts',(-18.6273802007938,4.21799814919381,13.));
#13618=CARTESIAN_POINT('Ctrl Pts',(-18.6095026819025,4.21040342106478,13.));
#13619=CARTESIAN_POINT('Ctrl Pts',(-18.5934584408283,4.20358750607481,13.));
#13620=CARTESIAN_POINT('Ctrl Pts',(-18.5773983084498,4.1968345819597,13.));
#13621=CARTESIAN_POINT('Ctrl Pts',(-18.5613135377966,4.19017810366012,13.));
#13622=CARTESIAN_POINT('Ctrl Pts',(-18.5444052403814,4.18318081925649,13.));
#13623=CARTESIAN_POINT('Ctrl Pts',(-18.5274697699072,4.17628995974216,13.));
#13624=CARTESIAN_POINT('Ctrl Pts',(-18.5104789585051,4.16960404100154,13.));
#13625=CARTESIAN_POINT('Ctrl Pts',(-18.482257258292,4.1584987447398,13.));
#13626=CARTESIAN_POINT('Ctrl Pts',(-18.4538805849791,4.14796697293776,13.));
#13627=CARTESIAN_POINT('Ctrl Pts',(-18.4251735639783,4.13860964459712,13.));
#13628=CARTESIAN_POINT('Ctrl Pts',(-18.4093434909438,4.13344968073196,13.));
#13629=CARTESIAN_POINT('Ctrl Pts',(-18.3934125378492,4.1286481456075,13.));
#13630=CARTESIAN_POINT('Ctrl Pts',(-18.377359006511,4.12427889810063,13.));
#13631=CARTESIAN_POINT('Ctrl Pts',(-18.3643002867397,4.12072474060085,13.));
#13632=CARTESIAN_POINT('Ctrl Pts',(-18.3511604736674,4.117456558433,13.));
#13633=CARTESIAN_POINT('Ctrl Pts',(-18.337935196262,4.11448919812531,13.));
#13634=CARTESIAN_POINT('',(-21.1275013067528,6.13422273260085,0.));
#13635=CARTESIAN_POINT('Origin',(-5.38923623413286E-12,1.75106900012182E-12,
0.));
#13636=CARTESIAN_POINT('',(-20.698113262342,7.45574324794401,0.));
#13637=CARTESIAN_POINT('Origin',(-5.38923623413286E-12,1.75106900012182E-12,
0.));
#13638=CARTESIAN_POINT('',(-20.698113262342,7.45574324794401,13.));
#13639=CARTESIAN_POINT('Origin',(-5.38923623413286E-12,1.75106900012182E-12,
13.));
#13640=CARTESIAN_POINT('',(-20.698113262342,7.45574324794401,0.));
#13641=CARTESIAN_POINT('Ctrl Pts',(-17.2541372868972,7.45007618140238,0.));
#13642=CARTESIAN_POINT('Ctrl Pts',(-17.2541372868972,7.45007618140238,21.));
#13643=CARTESIAN_POINT('Ctrl Pts',(-17.2627905583523,7.45381253347183,0.));
#13644=CARTESIAN_POINT('Ctrl Pts',(-17.2627905583523,7.45381253347183,21.));
#13645=CARTESIAN_POINT('Ctrl Pts',(-17.2801832097582,7.46105049818251,0.));
#13646=CARTESIAN_POINT('Ctrl Pts',(-17.2801832097582,7.46105049818251,21.));
#13647=CARTESIAN_POINT('Ctrl Pts',(-17.3065305096784,7.4712032346092,0.));
#13648=CARTESIAN_POINT('Ctrl Pts',(-17.3065305096784,7.4712032346092,21.));
#13649=CARTESIAN_POINT('Ctrl Pts',(-17.3421522689127,7.48340100912745,0.));
#13650=CARTESIAN_POINT('Ctrl Pts',(-17.3421522689127,7.48340100912745,21.));
#13651=CARTESIAN_POINT('Ctrl Pts',(-17.3873563447297,7.49681774451751,0.));
#13652=CARTESIAN_POINT('Ctrl Pts',(-17.3873563447297,7.49681774451751,21.));
#13653=CARTESIAN_POINT('Ctrl Pts',(-17.4330545448126,7.50891486634214,0.));
#13654=CARTESIAN_POINT('Ctrl Pts',(-17.4330545448126,7.50891486634214,21.));
#13655=CARTESIAN_POINT('Ctrl Pts',(-17.4790653226646,7.52019696747328,0.));
#13656=CARTESIAN_POINT('Ctrl Pts',(-17.4790653226646,7.52019696747328,21.));
#13657=CARTESIAN_POINT('Ctrl Pts',(-17.5252518287336,7.53103903007863,0.));
#13658=CARTESIAN_POINT('Ctrl Pts',(-17.5252518287336,7.53103903007863,21.));
#13659=CARTESIAN_POINT('Ctrl Pts',(-17.5715579419204,7.54158441095317,0.));
#13660=CARTESIAN_POINT('Ctrl Pts',(-17.5715579419204,7.54158441095317,21.));
#13661=CARTESIAN_POINT('Ctrl Pts',(-17.6179818599248,7.55182125346564,0.));
#13662=CARTESIAN_POINT('Ctrl Pts',(-17.6179818599248,7.55182125346564,21.));
#13663=CARTESIAN_POINT('Ctrl Pts',(-17.6645549117314,7.56164400295863,0.));
#13664=CARTESIAN_POINT('Ctrl Pts',(-17.6645549117314,7.56164400295863,21.));
#13665=CARTESIAN_POINT('Ctrl Pts',(-17.7113192869136,7.57091795530423,0.));
#13666=CARTESIAN_POINT('Ctrl Pts',(-17.7113192869136,7.57091795530423,21.));
#13667=CARTESIAN_POINT('Ctrl Pts',(-17.7583042294209,7.57954834582803,0.));
#13668=CARTESIAN_POINT('Ctrl Pts',(-17.7583042294209,7.57954834582803,21.));
#13669=CARTESIAN_POINT('Ctrl Pts',(-17.8055090348024,7.58752955799499,0.));
#13670=CARTESIAN_POINT('Ctrl Pts',(-17.8055090348024,7.58752955799499,21.));
#13671=CARTESIAN_POINT('Ctrl Pts',(-17.8529149331931,7.59491004201955,0.));
#13672=CARTESIAN_POINT('Ctrl Pts',(-17.8529149331931,7.59491004201955,21.));
#13673=CARTESIAN_POINT('Ctrl Pts',(-17.900492838997,7.60176928403058,0.));
#13674=CARTESIAN_POINT('Ctrl Pts',(-17.900492838997,7.60176928403058,21.));
#13675=CARTESIAN_POINT('Ctrl Pts',(-17.9482122228183,7.60819152580111,0.));
#13676=CARTESIAN_POINT('Ctrl Pts',(-17.9482122228183,7.60819152580111,21.));
#13677=CARTESIAN_POINT('Ctrl Pts',(-17.9960506269561,7.61423755067038,0.));
#13678=CARTESIAN_POINT('Ctrl Pts',(-17.9960506269561,7.61423755067038,21.));
#13679=CARTESIAN_POINT('Ctrl Pts',(-18.0439992897906,7.61992799636654,0.));
#13680=CARTESIAN_POINT('Ctrl Pts',(-18.0439992897906,7.61992799636654,21.));
#13681=CARTESIAN_POINT('Ctrl Pts',(-18.0920577897363,7.62525915358074,0.));
#13682=CARTESIAN_POINT('Ctrl Pts',(-18.0920577897363,7.62525915358074,21.));
#13683=CARTESIAN_POINT('Ctrl Pts',(-18.1402306858819,7.63021285851761,0.));
#13684=CARTESIAN_POINT('Ctrl Pts',(-18.1402306858819,7.63021285851761,21.));
#13685=CARTESIAN_POINT('Ctrl Pts',(-18.1885236169197,7.63476798969016,0.));
#13686=CARTESIAN_POINT('Ctrl Pts',(-18.1885236169197,7.63476798969016,21.));
#13687=CARTESIAN_POINT('Ctrl Pts',(-18.2369390502576,7.63891299603826,0.));
#13688=CARTESIAN_POINT('Ctrl Pts',(-18.2369390502576,7.63891299603826,21.));
#13689=CARTESIAN_POINT('Ctrl Pts',(-18.2854741391282,7.6426522027076,0.));
#13690=CARTESIAN_POINT('Ctrl Pts',(-18.2854741391282,7.6426522027076,21.));
#13691=CARTESIAN_POINT('Ctrl Pts',(-18.3341230095852,7.64599903846601,0.));
#13692=CARTESIAN_POINT('Ctrl Pts',(-18.3341230095852,7.64599903846601,21.));
#13693=CARTESIAN_POINT('Ctrl Pts',(-18.3828781275628,7.6489719793775,0.));
#13694=CARTESIAN_POINT('Ctrl Pts',(-18.3828781275628,7.6489719793775,21.));
#13695=CARTESIAN_POINT('Ctrl Pts',(-18.4317319183719,7.65158974829126,0.));
#13696=CARTESIAN_POINT('Ctrl Pts',(-18.4317319183719,7.65158974829126,21.));
#13697=CARTESIAN_POINT('Ctrl Pts',(-18.4806785483052,7.65386603444743,0.));
#13698=CARTESIAN_POINT('Ctrl Pts',(-18.4806785483052,7.65386603444743,21.));
#13699=CARTESIAN_POINT('Ctrl Pts',(-18.5297146894905,7.65580722110437,0.));
#13700=CARTESIAN_POINT('Ctrl Pts',(-18.5297146894905,7.65580722110437,21.));
#13701=CARTESIAN_POINT('Ctrl Pts',(-18.5788385228928,7.65741532450727,0.));
#13702=CARTESIAN_POINT('Ctrl Pts',(-18.5788385228928,7.65741532450727,21.));
#13703=CARTESIAN_POINT('Ctrl Pts',(-18.6280491346907,7.65868976978872,0.));
#13704=CARTESIAN_POINT('Ctrl Pts',(-18.6280491346907,7.65868976978872,21.));
#13705=CARTESIAN_POINT('Ctrl Pts',(-18.6773458057584,7.65962948375621,0.));
#13706=CARTESIAN_POINT('Ctrl Pts',(-18.6773458057584,7.65962948375621,21.));
#13707=CARTESIAN_POINT('Ctrl Pts',(-18.7267272235231,7.66023521705905,0.));
#13708=CARTESIAN_POINT('Ctrl Pts',(-18.7267272235231,7.66023521705905,21.));
#13709=CARTESIAN_POINT('Ctrl Pts',(-18.7761911671591,7.6605104692254,0.));
#13710=CARTESIAN_POINT('Ctrl Pts',(-18.7761911671591,7.6605104692254,21.));
#13711=CARTESIAN_POINT('Ctrl Pts',(-18.8257349246207,7.66046025294775,0.));
#13712=CARTESIAN_POINT('Ctrl Pts',(-18.8257349246207,7.66046025294775,21.));
#13713=CARTESIAN_POINT('Ctrl Pts',(-18.8753555389435,7.66009036321663,0.));
#13714=CARTESIAN_POINT('Ctrl Pts',(-18.8753555389435,7.66009036321663,21.));
#13715=CARTESIAN_POINT('Ctrl Pts',(-18.9250501008887,7.65940650980099,0.));
#13716=CARTESIAN_POINT('Ctrl Pts',(-18.9250501008887,7.65940650980099,21.));
#13717=CARTESIAN_POINT('Ctrl Pts',(-18.974816073814,7.65841335587266,0.));
#13718=CARTESIAN_POINT('Ctrl Pts',(-18.974816073814,7.65841335587266,21.));
#13719=CARTESIAN_POINT('Ctrl Pts',(-19.0246514144531,7.65711415727855,0.));
#13720=CARTESIAN_POINT('Ctrl Pts',(-19.0246514144531,7.65711415727855,21.));
#13721=CARTESIAN_POINT('Ctrl Pts',(-19.0745543888799,7.65551129907201,0.));
#13722=CARTESIAN_POINT('Ctrl Pts',(-19.0745543888799,7.65551129907201,21.));
#13723=CARTESIAN_POINT('Ctrl Pts',(-19.1245234597312,7.65360662280609,0.));
#13724=CARTESIAN_POINT('Ctrl Pts',(-19.1245234597312,7.65360662280609,21.));
#13725=CARTESIAN_POINT('Ctrl Pts',(-19.1745571539291,7.65140181220526,0.));
#13726=CARTESIAN_POINT('Ctrl Pts',(-19.1745571539291,7.65140181220526,21.));
#13727=CARTESIAN_POINT('Ctrl Pts',(-19.224653915265,7.64889882291923,0.));
#13728=CARTESIAN_POINT('Ctrl Pts',(-19.224653915265,7.64889882291923,21.));
#13729=CARTESIAN_POINT('Ctrl Pts',(-19.2748120456486,7.64610005549613,0.));
#13730=CARTESIAN_POINT('Ctrl Pts',(-19.2748120456486,7.64610005549613,21.));
#13731=CARTESIAN_POINT('Ctrl Pts',(-19.3250297839295,7.64300812875339,0.));
#13732=CARTESIAN_POINT('Ctrl Pts',(-19.3250297839295,7.64300812875339,21.));
#13733=CARTESIAN_POINT('Ctrl Pts',(-19.3753053524647,7.63962574822761,0.));
#13734=CARTESIAN_POINT('Ctrl Pts',(-19.3753053524647,7.63962574822761,21.));
#13735=CARTESIAN_POINT('Ctrl Pts',(-19.4256370121006,7.63595554930654,0.));
#13736=CARTESIAN_POINT('Ctrl Pts',(-19.4256370121006,7.63595554930654,21.));
#13737=CARTESIAN_POINT('Ctrl Pts',(-19.4760231231881,7.63199992715366,0.));
#13738=CARTESIAN_POINT('Ctrl Pts',(-19.4760231231881,7.63199992715366,21.));
#13739=CARTESIAN_POINT('Ctrl Pts',(-19.5264621687521,7.62776096538883,0.));
#13740=CARTESIAN_POINT('Ctrl Pts',(-19.5264621687521,7.62776096538883,21.));
#13741=CARTESIAN_POINT('Ctrl Pts',(-19.5769527121826,7.62324053735219,0.));
#13742=CARTESIAN_POINT('Ctrl Pts',(-19.5769527121826,7.62324053735219,21.));
#13743=CARTESIAN_POINT('Ctrl Pts',(-19.6274933688524,7.61844037070591,0.));
#13744=CARTESIAN_POINT('Ctrl Pts',(-19.6274933688524,7.61844037070591,21.));
#13745=CARTESIAN_POINT('Ctrl Pts',(-19.6780827744426,7.61336212350879,0.));
#13746=CARTESIAN_POINT('Ctrl Pts',(-19.6780827744426,7.61336212350879,21.));
#13747=CARTESIAN_POINT('Ctrl Pts',(-19.7287195480601,7.60800746969262,0.));
#13748=CARTESIAN_POINT('Ctrl Pts',(-19.7287195480601,7.60800746969262,21.));
#13749=CARTESIAN_POINT('Ctrl Pts',(-19.7794022782484,7.60237814110187,0.));
#13750=CARTESIAN_POINT('Ctrl Pts',(-19.7794022782484,7.60237814110187,21.));
#13751=CARTESIAN_POINT('Ctrl Pts',(-19.830129556152,7.59647587605448,0.));
#13752=CARTESIAN_POINT('Ctrl Pts',(-19.830129556152,7.59647587605448,21.));
#13753=CARTESIAN_POINT('Ctrl Pts',(-19.8808999994024,7.59030238888852,0.));
#13754=CARTESIAN_POINT('Ctrl Pts',(-19.8808999994024,7.59030238888852,21.));
#13755=CARTESIAN_POINT('Ctrl Pts',(-19.931712276832,7.58385933533352,0.));
#13756=CARTESIAN_POINT('Ctrl Pts',(-19.931712276832,7.58385933533352,21.));
#13757=CARTESIAN_POINT('Ctrl Pts',(-19.9825651387294,7.57714827622806,0.));
#13758=CARTESIAN_POINT('Ctrl Pts',(-19.9825651387294,7.57714827622806,21.));
#13759=CARTESIAN_POINT('Ctrl Pts',(-20.0334574248556,7.57017066105973,0.));
#13760=CARTESIAN_POINT('Ctrl Pts',(-20.0334574248556,7.57017066105973,21.));
#13761=CARTESIAN_POINT('Ctrl Pts',(-20.0843880130978,7.5629278654946,0.));
#13762=CARTESIAN_POINT('Ctrl Pts',(-20.0843880130978,7.5629278654946,21.));
#13763=CARTESIAN_POINT('Ctrl Pts',(-20.1353557774357,7.55542122125494,0.));
#13764=CARTESIAN_POINT('Ctrl Pts',(-20.1353557774357,7.55542122125494,21.));
#13765=CARTESIAN_POINT('Ctrl Pts',(-20.1863595454674,7.54765204869254,0.));
#13766=CARTESIAN_POINT('Ctrl Pts',(-20.1863595454674,7.54765204869254,21.));
#13767=CARTESIAN_POINT('Ctrl Pts',(-20.2373980474879,7.53962169534167,0.));
#13768=CARTESIAN_POINT('Ctrl Pts',(-20.2373980474879,7.53962169534167,21.));
#13769=CARTESIAN_POINT('Ctrl Pts',(-20.2884698940944,7.53133155804008,0.));
#13770=CARTESIAN_POINT('Ctrl Pts',(-20.2884698940944,7.53133155804008,21.));
#13771=CARTESIAN_POINT('Ctrl Pts',(-20.3395736743243,7.52278303006887,0.));
#13772=CARTESIAN_POINT('Ctrl Pts',(-20.3395736743243,7.52278303006887,21.));
#13773=CARTESIAN_POINT('Ctrl Pts',(-20.3907080367098,7.51397746081994,0.));
#13774=CARTESIAN_POINT('Ctrl Pts',(-20.3907080367098,7.51397746081994,21.));
#13775=CARTESIAN_POINT('Ctrl Pts',(-20.4418717748497,7.50491611266253,0.));
#13776=CARTESIAN_POINT('Ctrl Pts',(-20.4418717748497,7.50491611266253,21.));
#13777=CARTESIAN_POINT('Ctrl Pts',(-20.4930639156161,7.49560012018405,0.));
#13778=CARTESIAN_POINT('Ctrl Pts',(-20.4930639156161,7.49560012018405,21.));
#13779=CARTESIAN_POINT('Ctrl Pts',(-20.5442837929044,7.48603045196745,0.));
#13780=CARTESIAN_POINT('Ctrl Pts',(-20.5442837929044,7.48603045196745,21.));
#13781=CARTESIAN_POINT('Ctrl Pts',(-20.5955309838521,7.47620789245428,0.));
#13782=CARTESIAN_POINT('Ctrl Pts',(-20.5955309838521,7.47620789245428,21.));
#13783=CARTESIAN_POINT('Ctrl Pts',(-20.6365504027501,7.46814799701905,0.));
#13784=CARTESIAN_POINT('Ctrl Pts',(-20.6365504027501,7.46814799701905,21.));
#13785=CARTESIAN_POINT('Ctrl Pts',(-20.6673271112931,7.46198969876654,0.));
#13786=CARTESIAN_POINT('Ctrl Pts',(-20.6673271112931,7.46198969876654,21.));
#13787=CARTESIAN_POINT('Ctrl Pts',(-20.6878503127065,7.45783379370107,0.));
#13788=CARTESIAN_POINT('Ctrl Pts',(-20.6878503127065,7.45783379370107,21.));
#13789=CARTESIAN_POINT('Ctrl Pts',(-20.698113262342,7.45574324794401,0.));
#13790=CARTESIAN_POINT('Ctrl Pts',(-20.698113262342,7.45574324794401,21.));
#13791=CARTESIAN_POINT('Ctrl Pts',(-17.2541372868972,7.45007618140238,0.));
#13792=CARTESIAN_POINT('Ctrl Pts',(-17.2627905583523,7.45381253347183,0.));
#13793=CARTESIAN_POINT('Ctrl Pts',(-17.2801832097582,7.46105049818251,0.));
#13794=CARTESIAN_POINT('Ctrl Pts',(-17.3065305096784,7.4712032346092,0.));
#13795=CARTESIAN_POINT('Ctrl Pts',(-17.3421522689127,7.48340100912745,0.));
#13796=CARTESIAN_POINT('Ctrl Pts',(-17.3873563447297,7.49681774451751,0.));
#13797=CARTESIAN_POINT('Ctrl Pts',(-17.4330545448126,7.50891486634214,0.));
#13798=CARTESIAN_POINT('Ctrl Pts',(-17.4790653226646,7.52019696747328,0.));
#13799=CARTESIAN_POINT('Ctrl Pts',(-17.5252518287336,7.53103903007863,0.));
#13800=CARTESIAN_POINT('Ctrl Pts',(-17.5715579419204,7.54158441095317,0.));
#13801=CARTESIAN_POINT('Ctrl Pts',(-17.6179818599248,7.55182125346564,0.));
#13802=CARTESIAN_POINT('Ctrl Pts',(-17.6645549117314,7.56164400295863,0.));
#13803=CARTESIAN_POINT('Ctrl Pts',(-17.7113192869136,7.57091795530423,0.));
#13804=CARTESIAN_POINT('Ctrl Pts',(-17.7583042294209,7.57954834582803,0.));
#13805=CARTESIAN_POINT('Ctrl Pts',(-17.8055090348024,7.58752955799499,0.));
#13806=CARTESIAN_POINT('Ctrl Pts',(-17.8529149331931,7.59491004201955,0.));
#13807=CARTESIAN_POINT('Ctrl Pts',(-17.900492838997,7.60176928403058,0.));
#13808=CARTESIAN_POINT('Ctrl Pts',(-17.9482122228183,7.60819152580111,0.));
#13809=CARTESIAN_POINT('Ctrl Pts',(-17.9960506269561,7.61423755067038,0.));
#13810=CARTESIAN_POINT('Ctrl Pts',(-18.0439992897906,7.61992799636654,0.));
#13811=CARTESIAN_POINT('Ctrl Pts',(-18.0920577897363,7.62525915358074,0.));
#13812=CARTESIAN_POINT('Ctrl Pts',(-18.1402306858819,7.63021285851761,0.));
#13813=CARTESIAN_POINT('Ctrl Pts',(-18.1885236169197,7.63476798969016,0.));
#13814=CARTESIAN_POINT('Ctrl Pts',(-18.2369390502576,7.63891299603826,0.));
#13815=CARTESIAN_POINT('Ctrl Pts',(-18.2854741391282,7.6426522027076,0.));
#13816=CARTESIAN_POINT('Ctrl Pts',(-18.3341230095852,7.64599903846601,0.));
#13817=CARTESIAN_POINT('Ctrl Pts',(-18.3828781275628,7.6489719793775,0.));
#13818=CARTESIAN_POINT('Ctrl Pts',(-18.4317319183719,7.65158974829126,0.));
#13819=CARTESIAN_POINT('Ctrl Pts',(-18.4806785483052,7.65386603444743,0.));
#13820=CARTESIAN_POINT('Ctrl Pts',(-18.5297146894905,7.65580722110437,0.));
#13821=CARTESIAN_POINT('Ctrl Pts',(-18.5788385228928,7.65741532450727,0.));
#13822=CARTESIAN_POINT('Ctrl Pts',(-18.6280491346907,7.65868976978872,0.));
#13823=CARTESIAN_POINT('Ctrl Pts',(-18.6773458057584,7.65962948375621,0.));
#13824=CARTESIAN_POINT('Ctrl Pts',(-18.7267272235231,7.66023521705905,0.));
#13825=CARTESIAN_POINT('Ctrl Pts',(-18.7761911671591,7.6605104692254,0.));
#13826=CARTESIAN_POINT('Ctrl Pts',(-18.8257349246207,7.66046025294775,0.));
#13827=CARTESIAN_POINT('Ctrl Pts',(-18.8753555389435,7.66009036321663,0.));
#13828=CARTESIAN_POINT('Ctrl Pts',(-18.9250501008887,7.65940650980099,0.));
#13829=CARTESIAN_POINT('Ctrl Pts',(-18.974816073814,7.65841335587266,0.));
#13830=CARTESIAN_POINT('Ctrl Pts',(-19.0246514144531,7.65711415727855,0.));
#13831=CARTESIAN_POINT('Ctrl Pts',(-19.0745543888799,7.65551129907201,0.));
#13832=CARTESIAN_POINT('Ctrl Pts',(-19.1245234597312,7.65360662280609,0.));
#13833=CARTESIAN_POINT('Ctrl Pts',(-19.1745571539291,7.65140181220526,0.));
#13834=CARTESIAN_POINT('Ctrl Pts',(-19.224653915265,7.64889882291923,0.));
#13835=CARTESIAN_POINT('Ctrl Pts',(-19.2748120456486,7.64610005549613,0.));
#13836=CARTESIAN_POINT('Ctrl Pts',(-19.3250297839295,7.64300812875339,0.));
#13837=CARTESIAN_POINT('Ctrl Pts',(-19.3753053524647,7.63962574822761,0.));
#13838=CARTESIAN_POINT('Ctrl Pts',(-19.4256370121006,7.63595554930654,0.));
#13839=CARTESIAN_POINT('Ctrl Pts',(-19.4760231231881,7.63199992715366,0.));
#13840=CARTESIAN_POINT('Ctrl Pts',(-19.5264621687521,7.62776096538883,0.));
#13841=CARTESIAN_POINT('Ctrl Pts',(-19.5769527121826,7.62324053735219,0.));
#13842=CARTESIAN_POINT('Ctrl Pts',(-19.6274933688524,7.61844037070591,0.));
#13843=CARTESIAN_POINT('Ctrl Pts',(-19.6780827744426,7.61336212350879,0.));
#13844=CARTESIAN_POINT('Ctrl Pts',(-19.7287195480601,7.60800746969262,0.));
#13845=CARTESIAN_POINT('Ctrl Pts',(-19.7794022782484,7.60237814110187,0.));
#13846=CARTESIAN_POINT('Ctrl Pts',(-19.830129556152,7.59647587605448,0.));
#13847=CARTESIAN_POINT('Ctrl Pts',(-19.8808999994024,7.59030238888852,0.));
#13848=CARTESIAN_POINT('Ctrl Pts',(-19.931712276832,7.58385933533352,0.));
#13849=CARTESIAN_POINT('Ctrl Pts',(-19.9825651387294,7.57714827622806,0.));
#13850=CARTESIAN_POINT('Ctrl Pts',(-20.0334574248556,7.57017066105973,0.));
#13851=CARTESIAN_POINT('Ctrl Pts',(-20.0843880130978,7.5629278654946,0.));
#13852=CARTESIAN_POINT('Ctrl Pts',(-20.1353557774357,7.55542122125494,0.));
#13853=CARTESIAN_POINT('Ctrl Pts',(-20.1863595454674,7.54765204869254,0.));
#13854=CARTESIAN_POINT('Ctrl Pts',(-20.2373980474879,7.53962169534167,0.));
#13855=CARTESIAN_POINT('Ctrl Pts',(-20.2884698940944,7.53133155804008,0.));
#13856=CARTESIAN_POINT('Ctrl Pts',(-20.3395736743243,7.52278303006887,0.));
#13857=CARTESIAN_POINT('Ctrl Pts',(-20.3907080367098,7.51397746081994,0.));
#13858=CARTESIAN_POINT('Ctrl Pts',(-20.4418717748497,7.50491611266253,0.));
#13859=CARTESIAN_POINT('Ctrl Pts',(-20.4930639156161,7.49560012018405,0.));
#13860=CARTESIAN_POINT('Ctrl Pts',(-20.5545277683621,7.48411651832413,0.));
#13861=CARTESIAN_POINT('Ctrl Pts',(-20.6057817877246,7.47423073598682,0.));
#13862=CARTESIAN_POINT('Ctrl Pts',(-20.6468066077586,7.46612041736313,0.));
#13863=CARTESIAN_POINT('Ctrl Pts',(-20.6775873630604,7.45992433946825,0.));
#13864=CARTESIAN_POINT('Ctrl Pts',(-20.698113262342,7.45574324794401,0.));
#13865=CARTESIAN_POINT('Ctrl Pts',(-17.2541372868972,7.45007618140238,13.));
#13866=CARTESIAN_POINT('Ctrl Pts',(-17.2687220121555,7.45637364574105,13.));
#13867=CARTESIAN_POINT('Ctrl Pts',(-17.2834550499143,7.46226667104457,13.));
#13868=CARTESIAN_POINT('Ctrl Pts',(-17.2983267669271,7.46778231426201,13.));
#13869=CARTESIAN_POINT('Ctrl Pts',(-17.3157575316218,7.47424706066486,13.));
#13870=CARTESIAN_POINT('Ctrl Pts',(-17.3333785326358,7.48019417754631,13.));
#13871=CARTESIAN_POINT('Ctrl Pts',(-17.3511502187641,7.48573450281641,13.));
#13872=CARTESIAN_POINT('Ctrl Pts',(-17.3761558317125,7.49353000563545,13.));
#13873=CARTESIAN_POINT('Ctrl Pts',(-17.4014574303119,7.50052692940329,13.));
#13874=CARTESIAN_POINT('Ctrl Pts',(-17.4269165094344,7.50711117101308,13.));
#13875=CARTESIAN_POINT('Ctrl Pts',(-17.4438508122093,7.51149073008615,13.));
#13876=CARTESIAN_POINT('Ctrl Pts',(-17.4608540901245,7.51568961154121,13.));
#13877=CARTESIAN_POINT('Ctrl Pts',(-17.4778953549503,7.51979276933068,13.));
#13878=CARTESIAN_POINT('Ctrl Pts',(-17.4958340796436,7.52411201550815,13.));
#13879=CARTESIAN_POINT('Ctrl Pts',(-17.5138146001121,7.5283260217222,13.));
#13880=CARTESIAN_POINT('Ctrl Pts',(-17.5318219263245,7.53247314101481,13.));
#13881=CARTESIAN_POINT('Ctrl Pts',(-17.5518200478112,7.53707874400416,13.));
#13882=CARTESIAN_POINT('Ctrl Pts',(-17.5718516505879,7.54160061545662,13.));
#13883=CARTESIAN_POINT('Ctrl Pts',(-17.5919190740318,7.54602601378866,13.));
#13884=CARTESIAN_POINT('Ctrl Pts',(-17.6221716888658,7.55269751656531,13.));
#13885=CARTESIAN_POINT('Ctrl Pts',(-17.6525076946334,7.5591437511878,13.));
#13886=CARTESIAN_POINT('Ctrl Pts',(-17.6829731243182,7.56521559976737,13.));
#13887=CARTESIAN_POINT('Ctrl Pts',(-17.7051055929372,7.56962666501534,13.));
#13888=CARTESIAN_POINT('Ctrl Pts',(-17.7273074810734,7.57383703866986,13.));
#13889=CARTESIAN_POINT('Ctrl Pts',(-17.7495842479966,7.57782678310862,13.));
#13890=CARTESIAN_POINT('Ctrl Pts',(-17.7768156880398,7.5827039040502,13.));
#13891=CARTESIAN_POINT('Ctrl Pts',(-17.804158605046,7.58725254420512,13.));
#13892=CARTESIAN_POINT('Ctrl Pts',(-17.8315958504836,7.59151733245453,13.));
#13893=CARTESIAN_POINT('Ctrl Pts',(-17.8612326292062,7.59612401157375,13.));
#13894=CARTESIAN_POINT('Ctrl Pts',(-17.8909775513234,7.60040516925881,13.));
#13895=CARTESIAN_POINT('Ctrl Pts',(-17.9207992272113,7.60444696777764,13.));
#13896=CARTESIAN_POINT('Ctrl Pts',(-17.9483304583115,7.60817833718496,13.));
#13897=CARTESIAN_POINT('Ctrl Pts',(-17.9759263069947,7.61170808544359,13.));
#13898=CARTESIAN_POINT('Ctrl Pts',(-18.0035762489806,7.61506270604767,13.));
#13899=CARTESIAN_POINT('Ctrl Pts',(-18.0411401148566,7.61962013038154,13.));
#13900=CARTESIAN_POINT('Ctrl Pts',(-18.0788044381469,7.62385245909619,13.));
#13901=CARTESIAN_POINT('Ctrl Pts',(-18.1165756811382,7.62773031180927,13.));
#13902=CARTESIAN_POINT('Ctrl Pts',(-18.153024114841,7.63147235592348,13.));
#13903=CARTESIAN_POINT('Ctrl Pts',(-18.1895746221693,7.63487692332076,13.));
#13904=CARTESIAN_POINT('Ctrl Pts',(-18.2262298442069,7.63792794642771,13.));
#13905=CARTESIAN_POINT('Ctrl Pts',(-18.2760269903147,7.64207284679906,13.));
#13906=CARTESIAN_POINT('Ctrl Pts',(-18.3260163400117,7.64556831472679,13.));
#13907=CARTESIAN_POINT('Ctrl Pts',(-18.3761647741424,7.64849356609341,13.));
#13908=CARTESIAN_POINT('Ctrl Pts',(-18.4202441575899,7.65106479845398,13.));
#13909=CARTESIAN_POINT('Ctrl Pts',(-18.4644442731264,7.65320196597232,13.));
#13910=CARTESIAN_POINT('Ctrl Pts',(-18.5087513218291,7.65493429570773,13.));
#13911=CARTESIAN_POINT('Ctrl Pts',(-18.5740706685125,7.65748817031392,13.));
#13912=CARTESIAN_POINT('Ctrl Pts',(-18.6396252901455,7.65915358769466,13.));
#13913=CARTESIAN_POINT('Ctrl Pts',(-18.705403439408,7.65993127489916,13.));
#13914=CARTESIAN_POINT('Ctrl Pts',(-18.78841610566,7.66091272374015,13.));
#13915=CARTESIAN_POINT('Ctrl Pts',(-18.8717830756308,7.66048522719313,13.));
#13916=CARTESIAN_POINT('Ctrl Pts',(-18.9554457128649,7.65875983807032,13.));
#13917=CARTESIAN_POINT('Ctrl Pts',(-19.0687732052322,7.65642266547919,13.));
#13918=CARTESIAN_POINT('Ctrl Pts',(-19.1826450749315,7.65169843824091,13.));
#13919=CARTESIAN_POINT('Ctrl Pts',(-19.2969757397446,7.64469887385594,13.));
#13920=CARTESIAN_POINT('Ctrl Pts',(-19.3989045214534,7.63845857890604,13.));
#13921=CARTESIAN_POINT('Ctrl Pts',(-19.5011952233073,7.6304178474504,13.));
#13922=CARTESIAN_POINT('Ctrl Pts',(-19.6037897798545,7.62065725312474,13.));
#13923=CARTESIAN_POINT('Ctrl Pts',(-19.7491944792891,7.60682380686804,13.));
#13924=CARTESIAN_POINT('Ctrl Pts',(-19.8952104297527,7.5895301522803,13.));
#13925=CARTESIAN_POINT('Ctrl Pts',(-20.0416957588587,7.56895177443313,13.));
#13926=CARTESIAN_POINT('Ctrl Pts',(-20.1554820830514,7.55296697931836,13.));
#13927=CARTESIAN_POINT('Ctrl Pts',(-20.2695554960095,7.53499708015271,13.));
#13928=CARTESIAN_POINT('Ctrl Pts',(-20.38385017906,7.51511029031556,13.));
#13929=CARTESIAN_POINT('Ctrl Pts',(-20.4827237158978,7.49790671447922,13.));
#13930=CARTESIAN_POINT('Ctrl Pts',(-20.5817593973802,7.4792711652965,13.));
#13931=CARTESIAN_POINT('Ctrl Pts',(-20.6809436361476,7.45922687874239,13.));
#13932=CARTESIAN_POINT('Ctrl Pts',(-20.6866663413833,7.45807036894775,13.));
#13933=CARTESIAN_POINT('Ctrl Pts',(-20.6923895501261,7.45690915859471,13.));
#13934=CARTESIAN_POINT('Ctrl Pts',(-20.698113262342,7.45574324794401,13.));
#13935=CARTESIAN_POINT('Ctrl Pts',(-18.1978687191668,12.3627494547115,0.));
#13936=CARTESIAN_POINT('Ctrl Pts',(-18.1978687191668,12.3627494547115,21.));
#13937=CARTESIAN_POINT('Ctrl Pts',(-18.1935275957711,12.3532177620787,0.));
#13938=CARTESIAN_POINT('Ctrl Pts',(-18.1935275957711,12.3532177620787,21.));
#13939=CARTESIAN_POINT('Ctrl Pts',(-18.1848265584754,12.3341713636489,0.));
#13940=CARTESIAN_POINT('Ctrl Pts',(-18.1848265584754,12.3341713636489,21.));
#13941=CARTESIAN_POINT('Ctrl Pts',(-18.1717186310224,12.3056527265146,0.));
#13942=CARTESIAN_POINT('Ctrl Pts',(-18.1717186310224,12.3056527265146,21.));
#13943=CARTESIAN_POINT('Ctrl Pts',(-18.1541286139166,12.2677298318549,0.));
#13944=CARTESIAN_POINT('Ctrl Pts',(-18.1541286139166,12.2677298318549,21.));
#13945=CARTESIAN_POINT('Ctrl Pts',(-18.1319528884305,12.2204964278426,0.));
#13946=CARTESIAN_POINT('Ctrl Pts',(-18.1319528884305,12.2204964278426,21.));
#13947=CARTESIAN_POINT('Ctrl Pts',(-18.109588624154,12.1734337668195,0.));
#13948=CARTESIAN_POINT('Ctrl Pts',(-18.109588624154,12.1734337668195,21.));
#13949=CARTESIAN_POINT('Ctrl Pts',(-18.0870354350128,12.1265426519718,0.));
#13950=CARTESIAN_POINT('Ctrl Pts',(-18.0870354350128,12.1265426519718,21.));
#13951=CARTESIAN_POINT('Ctrl Pts',(-18.0642929289333,12.0798241915081,0.));
#13952=CARTESIAN_POINT('Ctrl Pts',(-18.0642929289333,12.0798241915081,21.));
#13953=CARTESIAN_POINT('Ctrl Pts',(-18.0413607600052,12.0332798395991,0.));
#13954=CARTESIAN_POINT('Ctrl Pts',(-18.0413607600052,12.0332798395991,21.));
#13955=CARTESIAN_POINT('Ctrl Pts',(-18.0182386160553,11.986911314246,0.));
#13956=CARTESIAN_POINT('Ctrl Pts',(-18.0182386160553,11.986911314246,21.));
#13957=CARTESIAN_POINT('Ctrl Pts',(-17.9949261997754,11.9407205019619,0.));
#13958=CARTESIAN_POINT('Ctrl Pts',(-17.9949261997754,11.9407205019619,21.));
#13959=CARTESIAN_POINT('Ctrl Pts',(-17.9714232133203,11.8947093631895,0.));
#13960=CARTESIAN_POINT('Ctrl Pts',(-17.9714232133203,11.8947093631895,21.));
#13961=CARTESIAN_POINT('Ctrl Pts',(-17.9477293432951,11.8488798430201,0.));
#13962=CARTESIAN_POINT('Ctrl Pts',(-17.9477293432951,11.8488798430201,21.));
#13963=CARTESIAN_POINT('Ctrl Pts',(-17.9238442458356,11.8032337607271,0.));
#13964=CARTESIAN_POINT('Ctrl Pts',(-17.9238442458356,11.8032337607271,21.));
#13965=CARTESIAN_POINT('Ctrl Pts',(-17.8997675418752,11.7577728408871,0.));
#13966=CARTESIAN_POINT('Ctrl Pts',(-17.8997675418752,11.7577728408871,21.));
#13967=CARTESIAN_POINT('Ctrl Pts',(-17.8754988158862,11.7124987772363,0.));
#13968=CARTESIAN_POINT('Ctrl Pts',(-17.8754988158862,11.7124987772363,21.));
#13969=CARTESIAN_POINT('Ctrl Pts',(-17.8510376144926,11.6674132861792,0.));
#13970=CARTESIAN_POINT('Ctrl Pts',(-17.8510376144926,11.6674132861792,21.));
#13971=CARTESIAN_POINT('Ctrl Pts',(-17.8263834470057,11.6225181583564,0.));
#13972=CARTESIAN_POINT('Ctrl Pts',(-17.8263834470057,11.6225181583564,21.));
#13973=CARTESIAN_POINT('Ctrl Pts',(-17.8015357852426,11.5778153222435,0.));
#13974=CARTESIAN_POINT('Ctrl Pts',(-17.8015357852426,11.5778153222435,21.));
#13975=CARTESIAN_POINT('Ctrl Pts',(-17.7764940721306,11.5333068279911,0.));
#13976=CARTESIAN_POINT('Ctrl Pts',(-17.7764940721306,11.5333068279911,21.));
#13977=CARTESIAN_POINT('Ctrl Pts',(-17.7512577332768,11.4889948016216,0.));
#13978=CARTESIAN_POINT('Ctrl Pts',(-17.7512577332768,11.4889948016216,21.));
#13979=CARTESIAN_POINT('Ctrl Pts',(-17.725826190457,11.4448814046804,0.));
#13980=CARTESIAN_POINT('Ctrl Pts',(-17.725826190457,11.4448814046804,21.));
#13981=CARTESIAN_POINT('Ctrl Pts',(-17.700198872213,11.4009687970126,0.));
#13982=CARTESIAN_POINT('Ctrl Pts',(-17.700198872213,11.4009687970126,21.));
#13983=CARTESIAN_POINT('Ctrl Pts',(-17.674375235974,11.3572590796967,0.));
#13984=CARTESIAN_POINT('Ctrl Pts',(-17.674375235974,11.3572590796967,21.));
#13985=CARTESIAN_POINT('Ctrl Pts',(-17.6483547422688,11.3137543310722,0.));
#13986=CARTESIAN_POINT('Ctrl Pts',(-17.6483547422688,11.3137543310722,21.));
#13987=CARTESIAN_POINT('Ctrl Pts',(-17.6221368072528,11.2704566868205,0.));
#13988=CARTESIAN_POINT('Ctrl Pts',(-17.6221368072528,11.2704566868205,21.));
#13989=CARTESIAN_POINT('Ctrl Pts',(-17.5957207597803,11.2273684103051,0.));
#13990=CARTESIAN_POINT('Ctrl Pts',(-17.5957207597803,11.2273684103051,21.));
#13991=CARTESIAN_POINT('Ctrl Pts',(-17.5691058058227,11.1844919535058,0.));
#13992=CARTESIAN_POINT('Ctrl Pts',(-17.5691058058227,11.1844919535058,21.));
#13993=CARTESIAN_POINT('Ctrl Pts',(-17.5422909714139,11.1418300507683,0.));
#13994=CARTESIAN_POINT('Ctrl Pts',(-17.5422909714139,11.1418300507683,21.));
#13995=CARTESIAN_POINT('Ctrl Pts',(-17.5152751467292,11.0993856581394,0.));
#13996=CARTESIAN_POINT('Ctrl Pts',(-17.5152751467292,11.0993856581394,21.));
#13997=CARTESIAN_POINT('Ctrl Pts',(-17.4880571878157,11.0571618040371,0.));
#13998=CARTESIAN_POINT('Ctrl Pts',(-17.4880571878157,11.0571618040371,21.));
#13999=CARTESIAN_POINT('Ctrl Pts',(-17.460636011184,11.0151614525642,0.));
#14000=CARTESIAN_POINT('Ctrl Pts',(-17.460636011184,11.0151614525642,21.));
#14001=CARTESIAN_POINT('Ctrl Pts',(-17.4330106728622,10.9733873885115,0.));
#14002=CARTESIAN_POINT('Ctrl Pts',(-17.4330106728622,10.9733873885115,21.));
#14003=CARTESIAN_POINT('Ctrl Pts',(-17.4051805054129,10.9318420203801,0.));
#14004=CARTESIAN_POINT('Ctrl Pts',(-17.4051805054129,10.9318420203801,21.));
#14005=CARTESIAN_POINT('Ctrl Pts',(-17.377145012528,10.8905275295837,0.));
#14006=CARTESIAN_POINT('Ctrl Pts',(-17.377145012528,10.8905275295837,21.));
#14007=CARTESIAN_POINT('Ctrl Pts',(-17.3489036079991,10.8494462423128,0.));
#14008=CARTESIAN_POINT('Ctrl Pts',(-17.3489036079991,10.8494462423128,21.));
#14009=CARTESIAN_POINT('Ctrl Pts',(-17.3204553814537,10.8086009632423,0.));
#14010=CARTESIAN_POINT('Ctrl Pts',(-17.3204553814537,10.8086009632423,21.));
#14011=CARTESIAN_POINT('Ctrl Pts',(-17.2917988998581,10.7679952591482,0.));
#14012=CARTESIAN_POINT('Ctrl Pts',(-17.2917988998581,10.7679952591482,21.));
#14013=CARTESIAN_POINT('Ctrl Pts',(-17.2629318816279,10.7276339231608,0.));
#14014=CARTESIAN_POINT('Ctrl Pts',(-17.2629318816279,10.7276339231608,21.));
#14015=CARTESIAN_POINT('Ctrl Pts',(-17.2338514174708,10.6875226650217,0.));
#14016=CARTESIAN_POINT('Ctrl Pts',(-17.2338514174708,10.6875226650217,21.));
#14017=CARTESIAN_POINT('Ctrl Pts',(-17.2045545572011,10.6476672831754,0.));
#14018=CARTESIAN_POINT('Ctrl Pts',(-17.2045545572011,10.6476672831754,21.));
#14019=CARTESIAN_POINT('Ctrl Pts',(-17.1750388395657,10.6080729180997,0.));
#14020=CARTESIAN_POINT('Ctrl Pts',(-17.1750388395657,10.6080729180997,21.));
#14021=CARTESIAN_POINT('Ctrl Pts',(-17.1453027387554,10.5687434234512,0.));
#14022=CARTESIAN_POINT('Ctrl Pts',(-17.1453027387554,10.5687434234512,21.));
#14023=CARTESIAN_POINT('Ctrl Pts',(-17.1153464189932,10.5296803023445,0.));
#14024=CARTESIAN_POINT('Ctrl Pts',(-17.1153464189932,10.5296803023445,21.));
#14025=CARTESIAN_POINT('Ctrl Pts',(-17.0851711712016,10.4908835057575,0.));
#14026=CARTESIAN_POINT('Ctrl Pts',(-17.0851711712016,10.4908835057575,21.));
#14027=CARTESIAN_POINT('Ctrl Pts',(-17.0547779975888,10.452353435089,0.));
#14028=CARTESIAN_POINT('Ctrl Pts',(-17.0547779975888,10.452353435089,21.));
#14029=CARTESIAN_POINT('Ctrl Pts',(-17.0241663361802,10.4140927470882,0.));
#14030=CARTESIAN_POINT('Ctrl Pts',(-17.0241663361802,10.4140927470882,21.));
#14031=CARTESIAN_POINT('Ctrl Pts',(-16.9933329788855,10.3761078860454,0.));
#14032=CARTESIAN_POINT('Ctrl Pts',(-16.9933329788855,10.3761078860454,21.));
#14033=CARTESIAN_POINT('Ctrl Pts',(-16.9622702798438,10.3384116178624,0.));
#14034=CARTESIAN_POINT('Ctrl Pts',(-16.9622702798438,10.3384116178624,21.));
#14035=CARTESIAN_POINT('Ctrl Pts',(-16.9309675442425,10.3010210756062,0.));
#14036=CARTESIAN_POINT('Ctrl Pts',(-16.9309675442425,10.3010210756062,21.));
#14037=CARTESIAN_POINT('Ctrl Pts',(-16.8994142530447,10.2639532144219,0.));
#14038=CARTESIAN_POINT('Ctrl Pts',(-16.8994142530447,10.2639532144219,21.));
#14039=CARTESIAN_POINT('Ctrl Pts',(-16.8676029947679,10.2272206796636,0.));
#14040=CARTESIAN_POINT('Ctrl Pts',(-16.8676029947679,10.2272206796636,21.));
#14041=CARTESIAN_POINT('Ctrl Pts',(-16.8355319435838,10.1908283166713,0.));
#14042=CARTESIAN_POINT('Ctrl Pts',(-16.8355319435838,10.1908283166713,21.));
#14043=CARTESIAN_POINT('Ctrl Pts',(-16.8032089941901,10.1547673397274,0.));
#14044=CARTESIAN_POINT('Ctrl Pts',(-16.8032089941901,10.1547673397274,21.));
#14045=CARTESIAN_POINT('Ctrl Pts',(-16.7706479198888,10.1190207721353,0.));
#14046=CARTESIAN_POINT('Ctrl Pts',(-16.7706479198888,10.1190207721353,21.));
#14047=CARTESIAN_POINT('Ctrl Pts',(-16.7378607357337,10.0835742491038,0.));
#14048=CARTESIAN_POINT('Ctrl Pts',(-16.7378607357337,10.0835742491038,21.));
#14049=CARTESIAN_POINT('Ctrl Pts',(-16.7048506904207,10.0484259314257,0.));
#14050=CARTESIAN_POINT('Ctrl Pts',(-16.7048506904207,10.0484259314257,21.));
#14051=CARTESIAN_POINT('Ctrl Pts',(-16.6716062376277,10.0135950379525,0.));
#14052=CARTESIAN_POINT('Ctrl Pts',(-16.6716062376277,10.0135950379525,21.));
#14053=CARTESIAN_POINT('Ctrl Pts',(-16.6380914029057,9.97913546489641,0.));
#14054=CARTESIAN_POINT('Ctrl Pts',(-16.6380914029057,9.97913546489641,21.));
#14055=CARTESIAN_POINT('Ctrl Pts',(-16.6042559779574,9.9451214271291,0.));
#14056=CARTESIAN_POINT('Ctrl Pts',(-16.6042559779574,9.9451214271291,21.));
#14057=CARTESIAN_POINT('Ctrl Pts',(-16.5700527532381,9.91162317616649,0.));
#14058=CARTESIAN_POINT('Ctrl Pts',(-16.5700527532381,9.91162317616649,21.));
#14059=CARTESIAN_POINT('Ctrl Pts',(-16.5354535643506,9.8786843754698,0.));
#14060=CARTESIAN_POINT('Ctrl Pts',(-16.5354535643506,9.8786843754698,21.));
#14061=CARTESIAN_POINT('Ctrl Pts',(-16.5004633692332,9.84630229363522,0.));
#14062=CARTESIAN_POINT('Ctrl Pts',(-16.5004633692332,9.84630229363522,21.));
#14063=CARTESIAN_POINT('Ctrl Pts',(-16.4651416449558,9.81439757053279,0.));
#14064=CARTESIAN_POINT('Ctrl Pts',(-16.4651416449558,9.81439757053279,21.));
#14065=CARTESIAN_POINT('Ctrl Pts',(-16.4295725710378,9.78285689698057,0.));
#14066=CARTESIAN_POINT('Ctrl Pts',(-16.4295725710378,9.78285689698057,21.));
#14067=CARTESIAN_POINT('Ctrl Pts',(-16.3938231282759,9.75159288382685,0.));
#14068=CARTESIAN_POINT('Ctrl Pts',(-16.3938231282759,9.75159288382685,21.));
#14069=CARTESIAN_POINT('Ctrl Pts',(-16.3579039682519,9.72060002001012,0.));
#14070=CARTESIAN_POINT('Ctrl Pts',(-16.3579039682519,9.72060002001012,21.));
#14071=CARTESIAN_POINT('Ctrl Pts',(-16.3217321000366,9.69000797146315,0.));
#14072=CARTESIAN_POINT('Ctrl Pts',(-16.3217321000366,9.69000797146315,21.));
#14073=CARTESIAN_POINT('Ctrl Pts',(-16.2850845948324,9.66014786078746,0.));
#14074=CARTESIAN_POINT('Ctrl Pts',(-16.2850845948324,9.66014786078746,21.));
#14075=CARTESIAN_POINT('Ctrl Pts',(-16.2476599387841,9.63146315443273,0.));
#14076=CARTESIAN_POINT('Ctrl Pts',(-16.2476599387841,9.63146315443273,21.));
#14077=CARTESIAN_POINT('Ctrl Pts',(-16.2168537871666,9.60981421781524,0.));
#14078=CARTESIAN_POINT('Ctrl Pts',(-16.2168537871666,9.60981421781524,21.));
#14079=CARTESIAN_POINT('Ctrl Pts',(-16.1931534965272,9.59446643316597,0.));
#14080=CARTESIAN_POINT('Ctrl Pts',(-16.1931534965272,9.59446643316597,21.));
#14081=CARTESIAN_POINT('Ctrl Pts',(-16.1770747160769,9.58464985151483,0.));
#14082=CARTESIAN_POINT('Ctrl Pts',(-16.1770747160769,9.58464985151483,21.));
#14083=CARTESIAN_POINT('Ctrl Pts',(-16.1689656784104,9.57984538049455,0.));
#14084=CARTESIAN_POINT('Ctrl Pts',(-16.1689656784104,9.57984538049455,21.));
#14085=CARTESIAN_POINT('',(-18.1978687191669,12.3627494547114,0.));
#14086=CARTESIAN_POINT('Ctrl Pts',(-16.1689656784104,9.57984538049455,0.));
#14087=CARTESIAN_POINT('Ctrl Pts',(-16.1770747160769,9.58464985151483,0.));
#14088=CARTESIAN_POINT('Ctrl Pts',(-16.1931534965272,9.59446643316597,0.));
#14089=CARTESIAN_POINT('Ctrl Pts',(-16.2168537871666,9.60981421781524,0.));
#14090=CARTESIAN_POINT('Ctrl Pts',(-16.2476599387841,9.63146315443273,0.));
#14091=CARTESIAN_POINT('Ctrl Pts',(-16.2850845948324,9.66014786078746,0.));
#14092=CARTESIAN_POINT('Ctrl Pts',(-16.3217321000366,9.69000797146315,0.));
#14093=CARTESIAN_POINT('Ctrl Pts',(-16.3579039682519,9.72060002001012,0.));
#14094=CARTESIAN_POINT('Ctrl Pts',(-16.3938231282759,9.75159288382685,0.));
#14095=CARTESIAN_POINT('Ctrl Pts',(-16.4295725710378,9.78285689698057,0.));
#14096=CARTESIAN_POINT('Ctrl Pts',(-16.4651416449558,9.81439757053279,0.));
#14097=CARTESIAN_POINT('Ctrl Pts',(-16.5004633692332,9.84630229363522,0.));
#14098=CARTESIAN_POINT('Ctrl Pts',(-16.5354535643506,9.8786843754698,0.));
#14099=CARTESIAN_POINT('Ctrl Pts',(-16.5700527532381,9.91162317616649,0.));
#14100=CARTESIAN_POINT('Ctrl Pts',(-16.6042559779574,9.9451214271291,0.));
#14101=CARTESIAN_POINT('Ctrl Pts',(-16.6380914029057,9.97913546489641,0.));
#14102=CARTESIAN_POINT('Ctrl Pts',(-16.6716062376277,10.0135950379525,0.));
#14103=CARTESIAN_POINT('Ctrl Pts',(-16.7048506904207,10.0484259314257,0.));
#14104=CARTESIAN_POINT('Ctrl Pts',(-16.7378607357337,10.0835742491038,0.));
#14105=CARTESIAN_POINT('Ctrl Pts',(-16.7706479198888,10.1190207721353,0.));
#14106=CARTESIAN_POINT('Ctrl Pts',(-16.8032089941901,10.1547673397274,0.));
#14107=CARTESIAN_POINT('Ctrl Pts',(-16.8355319435838,10.1908283166713,0.));
#14108=CARTESIAN_POINT('Ctrl Pts',(-16.8676029947679,10.2272206796636,0.));
#14109=CARTESIAN_POINT('Ctrl Pts',(-16.8994142530447,10.2639532144219,0.));
#14110=CARTESIAN_POINT('Ctrl Pts',(-16.9309675442425,10.3010210756062,0.));
#14111=CARTESIAN_POINT('Ctrl Pts',(-16.9622702798438,10.3384116178624,0.));
#14112=CARTESIAN_POINT('Ctrl Pts',(-16.9933329788855,10.3761078860454,0.));
#14113=CARTESIAN_POINT('Ctrl Pts',(-17.0241663361802,10.4140927470882,0.));
#14114=CARTESIAN_POINT('Ctrl Pts',(-17.0547779975888,10.452353435089,0.));
#14115=CARTESIAN_POINT('Ctrl Pts',(-17.0851711712016,10.4908835057575,0.));
#14116=CARTESIAN_POINT('Ctrl Pts',(-17.1153464189932,10.5296803023445,0.));
#14117=CARTESIAN_POINT('Ctrl Pts',(-17.1453027387554,10.5687434234512,0.));
#14118=CARTESIAN_POINT('Ctrl Pts',(-17.1750388395657,10.6080729180997,0.));
#14119=CARTESIAN_POINT('Ctrl Pts',(-17.2045545572011,10.6476672831754,0.));
#14120=CARTESIAN_POINT('Ctrl Pts',(-17.2338514174708,10.6875226650217,0.));
#14121=CARTESIAN_POINT('Ctrl Pts',(-17.2629318816279,10.7276339231608,0.));
#14122=CARTESIAN_POINT('Ctrl Pts',(-17.2917988998581,10.7679952591482,0.));
#14123=CARTESIAN_POINT('Ctrl Pts',(-17.3204553814537,10.8086009632423,0.));
#14124=CARTESIAN_POINT('Ctrl Pts',(-17.3489036079991,10.8494462423128,0.));
#14125=CARTESIAN_POINT('Ctrl Pts',(-17.377145012528,10.8905275295837,0.));
#14126=CARTESIAN_POINT('Ctrl Pts',(-17.4051805054129,10.9318420203801,0.));
#14127=CARTESIAN_POINT('Ctrl Pts',(-17.4330106728622,10.9733873885115,0.));
#14128=CARTESIAN_POINT('Ctrl Pts',(-17.460636011184,11.0151614525642,0.));
#14129=CARTESIAN_POINT('Ctrl Pts',(-17.4880571878157,11.0571618040371,0.));
#14130=CARTESIAN_POINT('Ctrl Pts',(-17.5152751467292,11.0993856581394,0.));
#14131=CARTESIAN_POINT('Ctrl Pts',(-17.5422909714139,11.1418300507683,0.));
#14132=CARTESIAN_POINT('Ctrl Pts',(-17.5691058058227,11.1844919535058,0.));
#14133=CARTESIAN_POINT('Ctrl Pts',(-17.5957207597803,11.2273684103051,0.));
#14134=CARTESIAN_POINT('Ctrl Pts',(-17.6221368072528,11.2704566868205,0.));
#14135=CARTESIAN_POINT('Ctrl Pts',(-17.6483547422688,11.3137543310722,0.));
#14136=CARTESIAN_POINT('Ctrl Pts',(-17.674375235974,11.3572590796967,0.));
#14137=CARTESIAN_POINT('Ctrl Pts',(-17.700198872213,11.4009687970126,0.));
#14138=CARTESIAN_POINT('Ctrl Pts',(-17.725826190457,11.4448814046804,0.));
#14139=CARTESIAN_POINT('Ctrl Pts',(-17.7512577332768,11.4889948016216,0.));
#14140=CARTESIAN_POINT('Ctrl Pts',(-17.7764940721306,11.5333068279911,0.));
#14141=CARTESIAN_POINT('Ctrl Pts',(-17.8015357852426,11.5778153222435,0.));
#14142=CARTESIAN_POINT('Ctrl Pts',(-17.8263834470057,11.6225181583564,0.));
#14143=CARTESIAN_POINT('Ctrl Pts',(-17.8510376144926,11.6674132861792,0.));
#14144=CARTESIAN_POINT('Ctrl Pts',(-17.8754988158862,11.7124987772363,0.));
#14145=CARTESIAN_POINT('Ctrl Pts',(-17.8997675418752,11.7577728408871,0.));
#14146=CARTESIAN_POINT('Ctrl Pts',(-17.9238442458356,11.8032337607271,0.));
#14147=CARTESIAN_POINT('Ctrl Pts',(-17.9477293432951,11.8488798430201,0.));
#14148=CARTESIAN_POINT('Ctrl Pts',(-17.9714232133203,11.8947093631895,0.));
#14149=CARTESIAN_POINT('Ctrl Pts',(-17.9949261997754,11.9407205019619,0.));
#14150=CARTESIAN_POINT('Ctrl Pts',(-18.0182386160553,11.986911314246,0.));
#14151=CARTESIAN_POINT('Ctrl Pts',(-18.0413607600052,12.0332798395991,0.));
#14152=CARTESIAN_POINT('Ctrl Pts',(-18.0642929289333,12.0798241915081,0.));
#14153=CARTESIAN_POINT('Ctrl Pts',(-18.0870354350128,12.1265426519718,0.));
#14154=CARTESIAN_POINT('Ctrl Pts',(-18.109588624154,12.1734337668195,0.));
#14155=CARTESIAN_POINT('Ctrl Pts',(-18.1364257412858,12.2299089600472,0.));
#14156=CARTESIAN_POINT('Ctrl Pts',(-18.1585543320743,12.2771850498068,0.));
#14157=CARTESIAN_POINT('Ctrl Pts',(-18.1761067306718,12.3151419520839,0.));
#14158=CARTESIAN_POINT('Ctrl Pts',(-18.1891864723772,12.3436860694314,0.));
#14159=CARTESIAN_POINT('Ctrl Pts',(-18.1978687191668,12.3627494547115,0.));
#14160=CARTESIAN_POINT('',(-18.1978687191669,12.3627494547114,13.));
#14161=CARTESIAN_POINT('Ctrl Pts',(-18.1978687191668,12.3627494547115,13.));
#14162=CARTESIAN_POINT('Ctrl Pts',(-18.1551298837072,12.2689088964153,13.));
#14163=CARTESIAN_POINT('Ctrl Pts',(-18.111299637656,12.1760519707549,13.));
#14164=CARTESIAN_POINT('Ctrl Pts',(-18.0663670681848,12.0842021157222,13.));
#14165=CARTESIAN_POINT('Ctrl Pts',(-17.9919118454842,11.9320029094011,13.));
#14166=CARTESIAN_POINT('Ctrl Pts',(-17.9144310022929,11.7825824042094,13.));
#14167=CARTESIAN_POINT('Ctrl Pts',(-17.8338669529311,11.6362239728201,13.));
#14168=CARTESIAN_POINT('Ctrl Pts',(-17.7719406994714,11.523724298462,13.));
#14169=CARTESIAN_POINT('Ctrl Pts',(-17.708190453754,11.4130324604454,13.));
#14170=CARTESIAN_POINT('Ctrl Pts',(-17.6425762029941,11.3042990938976,13.));
#14171=CARTESIAN_POINT('Ctrl Pts',(-17.571944040219,11.1872502400868,13.));
#14172=CARTESIAN_POINT('Ctrl Pts',(-17.499154807149,11.0724652191949,13.));
#14173=CARTESIAN_POINT('Ctrl Pts',(-17.4241207695605,10.9601920980076,13.));
#14174=CARTESIAN_POINT('Ctrl Pts',(-17.3825798919753,10.8980346540897,13.));
#14175=CARTESIAN_POINT('Ctrl Pts',(-17.3403540655037,10.8366430107889,13.));
#14176=CARTESIAN_POINT('Ctrl Pts',(-17.2974271318847,10.7760628634082,13.));
#14177=CARTESIAN_POINT('Ctrl Pts',(-17.2560610466519,10.71768544558,13.));
#14178=CARTESIAN_POINT('Ctrl Pts',(-17.2140399833079,10.6600671046061,13.));
#14179=CARTESIAN_POINT('Ctrl Pts',(-17.1713305004863,10.6032772242041,13.));
#14180=CARTESIAN_POINT('Ctrl Pts',(-17.1344164148599,10.5541933587631,13.));
#14181=CARTESIAN_POINT('Ctrl Pts',(-17.096989955235,10.5057257098335,13.));
#14182=CARTESIAN_POINT('Ctrl Pts',(-17.0590571075016,10.4578814177545,13.));
#14183=CARTESIAN_POINT('Ctrl Pts',(-17.0318344187272,10.423545733757,13.));
#14184=CARTESIAN_POINT('Ctrl Pts',(-17.004352569251,10.3895287972434,13.));
#14185=CARTESIAN_POINT('Ctrl Pts',(-16.9765917293735,10.3558648787318,13.));
#14186=CARTESIAN_POINT('Ctrl Pts',(-16.9492829411712,10.3227491363857,13.));
#14187=CARTESIAN_POINT('Ctrl Pts',(-16.9217004795811,10.2899802165512,13.));
#14188=CARTESIAN_POINT('Ctrl Pts',(-16.8938171684013,10.257603002843,13.));
#14189=CARTESIAN_POINT('Ctrl Pts',(-16.8696406992028,10.2295300560935,13.));
#14190=CARTESIAN_POINT('Ctrl Pts',(-16.8452366235594,10.2017536135352,13.));
#14191=CARTESIAN_POINT('Ctrl Pts',(-16.8206160301345,10.1742626909659,13.));
#14192=CARTESIAN_POINT('Ctrl Pts',(-16.7983154204895,10.1493622215735,13.));
#14193=CARTESIAN_POINT('Ctrl Pts',(-16.7758403904972,10.1246914564006,13.));
#14194=CARTESIAN_POINT('Ctrl Pts',(-16.7532063442149,10.1002324979069,13.));
#14195=CARTESIAN_POINT('Ctrl Pts',(-16.7341406196096,10.079629563683,13.));
#14196=CARTESIAN_POINT('Ctrl Pts',(-16.7149630708293,10.0591755003946,13.));
#14197=CARTESIAN_POINT('Ctrl Pts',(-16.6956634327229,10.0388873687047,13.));
#14198=CARTESIAN_POINT('Ctrl Pts',(-16.6677347574757,10.0095282357399,13.));
#14199=CARTESIAN_POINT('Ctrl Pts',(-16.6395499070626,9.98051721208624,13.));
#14200=CARTESIAN_POINT('Ctrl Pts',(-16.6109867038064,9.95203577377263,13.));
#14201=CARTESIAN_POINT('Ctrl Pts',(-16.5937277075416,9.9348261830604,13.));
#14202=CARTESIAN_POINT('Ctrl Pts',(-16.5763285722608,9.91781279953151,13.));
#14203=CARTESIAN_POINT('Ctrl Pts',(-16.5587751451304,9.90101792991858,13.));
#14204=CARTESIAN_POINT('Ctrl Pts',(-16.5425859473257,9.88552833553625,13.));
#14205=CARTESIAN_POINT('Ctrl Pts',(-16.5262647433908,9.87022569084434,13.));
#14206=CARTESIAN_POINT('Ctrl Pts',(-16.5098269904329,9.85509024411449,13.));
#14207=CARTESIAN_POINT('Ctrl Pts',(-16.4872151946467,9.83426990258338,13.));
#14208=CARTESIAN_POINT('Ctrl Pts',(-16.4643869859202,9.81375991310154,13.));
#14209=CARTESIAN_POINT('Ctrl Pts',(-16.4414328801903,9.7934396802235,13.));
#14210=CARTESIAN_POINT('Ctrl Pts',(-16.4268703865311,9.7805481624305,13.));
#14211=CARTESIAN_POINT('Ctrl Pts',(-16.4122582103724,9.76773166757831,13.));
#14212=CARTESIAN_POINT('Ctrl Pts',(-16.3976025796313,9.75498419478216,13.));
#14213=CARTESIAN_POINT('Ctrl Pts',(-16.3844498331849,9.74354393127652,13.));
#14214=CARTESIAN_POINT('Ctrl Pts',(-16.3712625079592,9.73215866496981,13.));
#14215=CARTESIAN_POINT('Ctrl Pts',(-16.3580219469452,9.72085751043954,13.));
#14216=CARTESIAN_POINT('Ctrl Pts',(-16.3441034802572,9.70897774622862,13.));
#14217=CARTESIAN_POINT('Ctrl Pts',(-16.330126283354,9.69719080116679,13.));
#14218=CARTESIAN_POINT('Ctrl Pts',(-16.3160331239166,9.68558166507924,13.));
#14219=CARTESIAN_POINT('Ctrl Pts',(-16.292624417431,9.66629891585391,13.));
#14220=CARTESIAN_POINT('Ctrl Pts',(-16.268891093964,9.64751373148189,13.));
#14221=CARTESIAN_POINT('Ctrl Pts',(-16.2444806681934,9.62974342615828,13.));
#14222=CARTESIAN_POINT('Ctrl Pts',(-16.231019890619,9.61994424733045,13.));
#14223=CARTESIAN_POINT('Ctrl Pts',(-16.2173524098339,9.61045478083913,13.));
#14224=CARTESIAN_POINT('Ctrl Pts',(-16.2034347659916,9.60133856554245,13.));
#14225=CARTESIAN_POINT('Ctrl Pts',(-16.1921134806533,9.59392299464928,13.));
#14226=CARTESIAN_POINT('Ctrl Pts',(-16.1806266997688,9.58675434324541,13.));
#14227=CARTESIAN_POINT('Ctrl Pts',(-16.1689656784104,9.57984538049455,13.));
#14228=CARTESIAN_POINT('',(-18.1978687191669,12.3627494547114,0.));
#14229=CARTESIAN_POINT('Origin',(-4.58435815896522E-12,3.33073116609659E-12,
0.));
#14230=CARTESIAN_POINT('',(-17.3811241238545,13.4869019493419,0.));
#14231=CARTESIAN_POINT('Origin',(-4.58435815896522E-12,3.33073116609659E-12,
0.));
#14232=CARTESIAN_POINT('',(-17.3811241238545,13.4869019493419,13.));
#14233=CARTESIAN_POINT('Origin',(-4.58435815896522E-12,3.33073116609659E-12,
13.));
#14234=CARTESIAN_POINT('',(-17.3811241238545,13.4869019493419,0.));
#14235=CARTESIAN_POINT('Ctrl Pts',(-14.1074595503134,12.4172651441477,0.));
#14236=CARTESIAN_POINT('Ctrl Pts',(-14.1074595503134,12.4172651441477,21.));
#14237=CARTESIAN_POINT('Ctrl Pts',(-14.1145347042316,12.4234926340671,0.));
#14238=CARTESIAN_POINT('Ctrl Pts',(-14.1145347042316,12.4234926340671,21.));
#14239=CARTESIAN_POINT('Ctrl Pts',(-14.1288394445866,12.4357509724316,0.));
#14240=CARTESIAN_POINT('Ctrl Pts',(-14.1288394445866,12.4357509724316,21.));
#14241=CARTESIAN_POINT('Ctrl Pts',(-14.1507598477672,12.4535485619996,0.));
#14242=CARTESIAN_POINT('Ctrl Pts',(-14.1507598477672,12.4535485619996,21.));
#14243=CARTESIAN_POINT('Ctrl Pts',(-14.1808688343892,12.4761570639125,0.));
#14244=CARTESIAN_POINT('Ctrl Pts',(-14.1808688343892,12.4761570639125,21.));
#14245=CARTESIAN_POINT('Ctrl Pts',(-14.2197144660135,12.5028859651751,0.));
#14246=CARTESIAN_POINT('Ctrl Pts',(-14.2197144660135,12.5028859651751,21.));
#14247=CARTESIAN_POINT('Ctrl Pts',(-14.2594378207584,12.5285125321527,0.));
#14248=CARTESIAN_POINT('Ctrl Pts',(-14.2594378207584,12.5285125321527,21.));
#14249=CARTESIAN_POINT('Ctrl Pts',(-14.2997103098726,12.5534605602317,0.));
#14250=CARTESIAN_POINT('Ctrl Pts',(-14.2997103098726,12.5534605602317,21.));
#14251=CARTESIAN_POINT('Ctrl Pts',(-14.3402859058353,12.5780443898087,0.));
#14252=CARTESIAN_POINT('Ctrl Pts',(-14.3402859058353,12.5780443898087,21.));
#14253=CARTESIAN_POINT('Ctrl Pts',(-14.3810669346235,12.6023830189244,0.));
#14254=CARTESIAN_POINT('Ctrl Pts',(-14.3810669346235,12.6023830189244,21.));
#14255=CARTESIAN_POINT('Ctrl Pts',(-14.4220553460485,12.626464614311,0.));
#14256=CARTESIAN_POINT('Ctrl Pts',(-14.4220553460485,12.626464614311,21.));
#14257=CARTESIAN_POINT('Ctrl Pts',(-14.463313553928,12.6501984687124,0.));
#14258=CARTESIAN_POINT('Ctrl Pts',(-14.463313553928,12.6501984687124,21.));
#14259=CARTESIAN_POINT('Ctrl Pts',(-14.5049233087958,12.6734695081852,0.));
#14260=CARTESIAN_POINT('Ctrl Pts',(-14.5049233087958,12.6734695081852,21.));
#14261=CARTESIAN_POINT('Ctrl Pts',(-14.5469417071951,12.6961966430455,0.));
#14262=CARTESIAN_POINT('Ctrl Pts',(-14.5469417071951,12.6961966430455,21.));
#14263=CARTESIAN_POINT('Ctrl Pts',(-14.5893698147583,12.7183743139638,0.));
#14264=CARTESIAN_POINT('Ctrl Pts',(-14.5893698147583,12.7183743139638,21.));
#14265=CARTESIAN_POINT('Ctrl Pts',(-14.6321748083434,12.7400427996251,0.));
#14266=CARTESIAN_POINT('Ctrl Pts',(-14.6321748083434,12.7400427996251,21.));
#14267=CARTESIAN_POINT('Ctrl Pts',(-14.6753044633399,12.7612687078867,0.));
#14268=CARTESIAN_POINT('Ctrl Pts',(-14.6753044633399,12.7612687078867,21.));
#14269=CARTESIAN_POINT('Ctrl Pts',(-14.7187037124277,12.7821227233337,0.));
#14270=CARTESIAN_POINT('Ctrl Pts',(-14.7187037124277,12.7821227233337,21.));
#14271=CARTESIAN_POINT('Ctrl Pts',(-14.7623324139791,12.8026557145457,0.));
#14272=CARTESIAN_POINT('Ctrl Pts',(-14.7623324139791,12.8026557145457,21.));
#14273=CARTESIAN_POINT('Ctrl Pts',(-14.8061758577898,12.8228846016791,0.));
#14274=CARTESIAN_POINT('Ctrl Pts',(-14.8061758577898,12.8228846016791,21.));
#14275=CARTESIAN_POINT('Ctrl Pts',(-14.8502347891476,12.8428057266944,0.));
#14276=CARTESIAN_POINT('Ctrl Pts',(-14.8502347891476,12.8428057266944,21.));
#14277=CARTESIAN_POINT('Ctrl Pts',(-14.8945191569251,12.8624032236317,0.));
#14278=CARTESIAN_POINT('Ctrl Pts',(-14.8945191569251,12.8624032236317,21.));
#14279=CARTESIAN_POINT('Ctrl Pts',(-14.9390408507356,12.8816587472147,0.));
#14280=CARTESIAN_POINT('Ctrl Pts',(-14.9390408507356,12.8816587472147,21.));
#14281=CARTESIAN_POINT('Ctrl Pts',(-14.9838057866976,12.9005620742036,0.));
#14282=CARTESIAN_POINT('Ctrl Pts',(-14.9838057866976,12.9005620742036,21.));
#14283=CARTESIAN_POINT('Ctrl Pts',(-15.0288099208306,12.9191164383568,0.));
#14284=CARTESIAN_POINT('Ctrl Pts',(-15.0288099208306,12.9191164383568,21.));
#14285=CARTESIAN_POINT('Ctrl Pts',(-15.0740435169624,12.9373327960422,0.));
#14286=CARTESIAN_POINT('Ctrl Pts',(-15.0740435169624,12.9373327960422,21.));
#14287=CARTESIAN_POINT('Ctrl Pts',(-15.1194937003528,12.9552263908864,0.));
#14288=CARTESIAN_POINT('Ctrl Pts',(-15.1194937003528,12.9552263908864,21.));
#14289=CARTESIAN_POINT('Ctrl Pts',(-15.1651474813659,12.9728126886697,0.));
#14290=CARTESIAN_POINT('Ctrl Pts',(-15.1651474813659,12.9728126886697,21.));
#14291=CARTESIAN_POINT('Ctrl Pts',(-15.2109950816083,12.9901029059182,0.));
#14292=CARTESIAN_POINT('Ctrl Pts',(-15.2109950816083,12.9901029059182,21.));
#14293=CARTESIAN_POINT('Ctrl Pts',(-15.2570313635503,13.0071020851025,0.));
#14294=CARTESIAN_POINT('Ctrl Pts',(-15.2570313635503,13.0071020851025,21.));
#14295=CARTESIAN_POINT('Ctrl Pts',(-15.3032539741328,13.0238115816728,0.));
#14296=CARTESIAN_POINT('Ctrl Pts',(-15.3032539741328,13.0238115816728,21.));
#14297=CARTESIAN_POINT('Ctrl Pts',(-15.3496622219036,13.0402305665115,0.));
#14298=CARTESIAN_POINT('Ctrl Pts',(-15.3496622219036,13.0402305665115,21.));
#14299=CARTESIAN_POINT('Ctrl Pts',(-15.3962557545684,13.0563577967298,0.));
#14300=CARTESIAN_POINT('Ctrl Pts',(-15.3962557545684,13.0563577967298,21.));
#14301=CARTESIAN_POINT('Ctrl Pts',(-15.4430330918328,13.0721935806302,0.));
#14302=CARTESIAN_POINT('Ctrl Pts',(-15.4430330918328,13.0721935806302,21.));
#14303=CARTESIAN_POINT('Ctrl Pts',(-15.4899910401523,13.087740560189,0.));
#14304=CARTESIAN_POINT('Ctrl Pts',(-15.4899910401523,13.087740560189,21.));
#14305=CARTESIAN_POINT('Ctrl Pts',(-15.5371254712111,13.1030026646917,0.));
#14306=CARTESIAN_POINT('Ctrl Pts',(-15.5371254712111,13.1030026646917,21.));
#14307=CARTESIAN_POINT('Ctrl Pts',(-15.5844317820184,13.1179844917497,0.));
#14308=CARTESIAN_POINT('Ctrl Pts',(-15.5844317820184,13.1179844917497,21.));
#14309=CARTESIAN_POINT('Ctrl Pts',(-15.6319054413079,13.1326905726717,0.));
#14310=CARTESIAN_POINT('Ctrl Pts',(-15.6319054413079,13.1326905726717,21.));
#14311=CARTESIAN_POINT('Ctrl Pts',(-15.6795425955901,13.147124558532,0.));
#14312=CARTESIAN_POINT('Ctrl Pts',(-15.6795425955901,13.147124558532,21.));
#14313=CARTESIAN_POINT('Ctrl Pts',(-15.7273402954914,13.161288914421,0.));
#14314=CARTESIAN_POINT('Ctrl Pts',(-15.7273402954914,13.161288914421,21.));
#14315=CARTESIAN_POINT('Ctrl Pts',(-15.7752961549278,13.1751853728467,0.));
#14316=CARTESIAN_POINT('Ctrl Pts',(-15.7752961549278,13.1751853728467,21.));
#14317=CARTESIAN_POINT('Ctrl Pts',(-15.8234081427091,13.1888152101588,0.));
#14318=CARTESIAN_POINT('Ctrl Pts',(-15.8234081427091,13.1888152101588,21.));
#14319=CARTESIAN_POINT('Ctrl Pts',(-15.8716743375555,13.2021795724682,0.));
#14320=CARTESIAN_POINT('Ctrl Pts',(-15.8716743375555,13.2021795724682,21.));
#14321=CARTESIAN_POINT('Ctrl Pts',(-15.9200926550954,13.2152798388134,0.));
#14322=CARTESIAN_POINT('Ctrl Pts',(-15.9200926550954,13.2152798388134,21.));
#14323=CARTESIAN_POINT('Ctrl Pts',(-15.9686607385389,13.2281177675127,0.));
#14324=CARTESIAN_POINT('Ctrl Pts',(-15.9686607385389,13.2281177675127,21.));
#14325=CARTESIAN_POINT('Ctrl Pts',(-16.0173761036734,13.240695304984,0.));
#14326=CARTESIAN_POINT('Ctrl Pts',(-16.0173761036734,13.240695304984,21.));
#14327=CARTESIAN_POINT('Ctrl Pts',(-16.0662362238032,13.2530144750236,0.));
#14328=CARTESIAN_POINT('Ctrl Pts',(-16.0662362238032,13.2530144750236,21.));
#14329=CARTESIAN_POINT('Ctrl Pts',(-16.1152386305152,13.2650772466062,0.));
#14330=CARTESIAN_POINT('Ctrl Pts',(-16.1152386305152,13.2650772466062,21.));
#14331=CARTESIAN_POINT('Ctrl Pts',(-16.1643810242643,13.2768853909882,0.));
#14332=CARTESIAN_POINT('Ctrl Pts',(-16.1643810242643,13.2768853909882,21.));
#14333=CARTESIAN_POINT('Ctrl Pts',(-16.2136613184475,13.2884404210388,0.));
#14334=CARTESIAN_POINT('Ctrl Pts',(-16.2136613184475,13.2884404210388,21.));
#14335=CARTESIAN_POINT('Ctrl Pts',(-16.2630775678735,13.2997436744733,0.));
#14336=CARTESIAN_POINT('Ctrl Pts',(-16.2630775678735,13.2997436744733,21.));
#14337=CARTESIAN_POINT('Ctrl Pts',(-16.3126279218067,13.3107963665229,0.));
#14338=CARTESIAN_POINT('Ctrl Pts',(-16.3126279218067,13.3107963665229,21.));
#14339=CARTESIAN_POINT('Ctrl Pts',(-16.3623105703343,13.3215996524974,0.));
#14340=CARTESIAN_POINT('Ctrl Pts',(-16.3623105703343,13.3215996524974,21.));
#14341=CARTESIAN_POINT('Ctrl Pts',(-16.4121236828756,13.3321546976812,0.));
#14342=CARTESIAN_POINT('Ctrl Pts',(-16.4121236828756,13.3321546976812,21.));
#14343=CARTESIAN_POINT('Ctrl Pts',(-16.4620653818862,13.3424627129921,0.));
#14344=CARTESIAN_POINT('Ctrl Pts',(-16.4620653818862,13.3424627129921,21.));
#14345=CARTESIAN_POINT('Ctrl Pts',(-16.5121337902953,13.3525249163084,0.));
#14346=CARTESIAN_POINT('Ctrl Pts',(-16.5121337902953,13.3525249163084,21.));
#14347=CARTESIAN_POINT('Ctrl Pts',(-16.5623270636327,13.3623425108873,0.));
#14348=CARTESIAN_POINT('Ctrl Pts',(-16.5623270636327,13.3623425108873,21.));
#14349=CARTESIAN_POINT('Ctrl Pts',(-16.612643424234,13.3719166600676,0.));
#14350=CARTESIAN_POINT('Ctrl Pts',(-16.612643424234,13.3719166600676,21.));
#14351=CARTESIAN_POINT('Ctrl Pts',(-16.6630812012276,13.381248462113,0.));
#14352=CARTESIAN_POINT('Ctrl Pts',(-16.6630812012276,13.381248462113,21.));
#14353=CARTESIAN_POINT('Ctrl Pts',(-16.7136388432444,13.3903389370346,0.));
#14354=CARTESIAN_POINT('Ctrl Pts',(-16.7136388432444,13.3903389370346,21.));
#14355=CARTESIAN_POINT('Ctrl Pts',(-16.7643148579872,13.3991890464165,0.));
#14356=CARTESIAN_POINT('Ctrl Pts',(-16.7643148579872,13.3991890464165,21.));
#14357=CARTESIAN_POINT('Ctrl Pts',(-16.8151077630226,13.4077997088426,0.));
#14358=CARTESIAN_POINT('Ctrl Pts',(-16.8151077630226,13.4077997088426,21.));
#14359=CARTESIAN_POINT('Ctrl Pts',(-16.8660160353187,13.4161718177499,0.));
#14360=CARTESIAN_POINT('Ctrl Pts',(-16.8660160353187,13.4161718177499,21.));
#14361=CARTESIAN_POINT('Ctrl Pts',(-16.9170380509036,13.4243062623592,0.));
#14362=CARTESIAN_POINT('Ctrl Pts',(-16.9170380509036,13.4243062623592,21.));
#14363=CARTESIAN_POINT('Ctrl Pts',(-16.9681720567298,13.432203941793,0.));
#14364=CARTESIAN_POINT('Ctrl Pts',(-16.9681720567298,13.432203941793,21.));
#14365=CARTESIAN_POINT('Ctrl Pts',(-17.0194162803447,13.4398657451291,0.));
#14366=CARTESIAN_POINT('Ctrl Pts',(-17.0194162803447,13.4398657451291,21.));
#14367=CARTESIAN_POINT('Ctrl Pts',(-17.0707690194411,13.4472925380889,0.));
#14368=CARTESIAN_POINT('Ctrl Pts',(-17.0707690194411,13.4472925380889,21.));
#14369=CARTESIAN_POINT('Ctrl Pts',(-17.1222287365697,13.4544851484583,0.));
#14370=CARTESIAN_POINT('Ctrl Pts',(-17.1222287365697,13.4544851484583,21.));
#14371=CARTESIAN_POINT('Ctrl Pts',(-17.1737941556239,13.4614443545811,0.));
#14372=CARTESIAN_POINT('Ctrl Pts',(-17.1737941556239,13.4614443545811,21.));
#14373=CARTESIAN_POINT('Ctrl Pts',(-17.2254643437923,13.4681708717969,0.));
#14374=CARTESIAN_POINT('Ctrl Pts',(-17.2254643437923,13.4681708717969,21.));
#14375=CARTESIAN_POINT('Ctrl Pts',(-17.2772386565028,13.474665315482,0.));
#14376=CARTESIAN_POINT('Ctrl Pts',(-17.2772386565028,13.474665315482,21.));
#14377=CARTESIAN_POINT('Ctrl Pts',(-17.3187410868027,13.4796755969465,0.));
#14378=CARTESIAN_POINT('Ctrl Pts',(-17.3187410868027,13.4796755969465,21.));
#14379=CARTESIAN_POINT('Ctrl Pts',(-17.3499144948292,13.4833292332349,0.));
#14380=CARTESIAN_POINT('Ctrl Pts',(-17.3499144948292,13.4833292332349,21.));
#14381=CARTESIAN_POINT('Ctrl Pts',(-17.3707174645609,13.485718750657,0.));
#14382=CARTESIAN_POINT('Ctrl Pts',(-17.3707174645609,13.485718750657,21.));
#14383=CARTESIAN_POINT('Ctrl Pts',(-17.3811241238545,13.4869019493419,0.));
#14384=CARTESIAN_POINT('Ctrl Pts',(-17.3811241238545,13.4869019493419,21.));
#14385=CARTESIAN_POINT('Ctrl Pts',(-14.1074595503134,12.4172651441477,0.));
#14386=CARTESIAN_POINT('Ctrl Pts',(-14.1145347042316,12.4234926340671,0.));
#14387=CARTESIAN_POINT('Ctrl Pts',(-14.1288394445866,12.4357509724316,0.));
#14388=CARTESIAN_POINT('Ctrl Pts',(-14.1507598477672,12.4535485619996,0.));
#14389=CARTESIAN_POINT('Ctrl Pts',(-14.1808688343892,12.4761570639125,0.));
#14390=CARTESIAN_POINT('Ctrl Pts',(-14.2197144660135,12.5028859651751,0.));
#14391=CARTESIAN_POINT('Ctrl Pts',(-14.2594378207584,12.5285125321527,0.));
#14392=CARTESIAN_POINT('Ctrl Pts',(-14.2997103098726,12.5534605602317,0.));
#14393=CARTESIAN_POINT('Ctrl Pts',(-14.3402859058353,12.5780443898087,0.));
#14394=CARTESIAN_POINT('Ctrl Pts',(-14.3810669346235,12.6023830189244,0.));
#14395=CARTESIAN_POINT('Ctrl Pts',(-14.4220553460485,12.626464614311,0.));
#14396=CARTESIAN_POINT('Ctrl Pts',(-14.463313553928,12.6501984687124,0.));
#14397=CARTESIAN_POINT('Ctrl Pts',(-14.5049233087958,12.6734695081852,0.));
#14398=CARTESIAN_POINT('Ctrl Pts',(-14.5469417071951,12.6961966430455,0.));
#14399=CARTESIAN_POINT('Ctrl Pts',(-14.5893698147583,12.7183743139638,0.));
#14400=CARTESIAN_POINT('Ctrl Pts',(-14.6321748083434,12.7400427996251,0.));
#14401=CARTESIAN_POINT('Ctrl Pts',(-14.6753044633399,12.7612687078867,0.));
#14402=CARTESIAN_POINT('Ctrl Pts',(-14.7187037124277,12.7821227233337,0.));
#14403=CARTESIAN_POINT('Ctrl Pts',(-14.7623324139791,12.8026557145457,0.));
#14404=CARTESIAN_POINT('Ctrl Pts',(-14.8061758577898,12.8228846016791,0.));
#14405=CARTESIAN_POINT('Ctrl Pts',(-14.8502347891476,12.8428057266944,0.));
#14406=CARTESIAN_POINT('Ctrl Pts',(-14.8945191569251,12.8624032236317,0.));
#14407=CARTESIAN_POINT('Ctrl Pts',(-14.9390408507356,12.8816587472147,0.));
#14408=CARTESIAN_POINT('Ctrl Pts',(-14.9838057866976,12.9005620742036,0.));
#14409=CARTESIAN_POINT('Ctrl Pts',(-15.0288099208306,12.9191164383568,0.));
#14410=CARTESIAN_POINT('Ctrl Pts',(-15.0740435169624,12.9373327960422,0.));
#14411=CARTESIAN_POINT('Ctrl Pts',(-15.1194937003528,12.9552263908864,0.));
#14412=CARTESIAN_POINT('Ctrl Pts',(-15.1651474813659,12.9728126886697,0.));
#14413=CARTESIAN_POINT('Ctrl Pts',(-15.2109950816083,12.9901029059182,0.));
#14414=CARTESIAN_POINT('Ctrl Pts',(-15.2570313635503,13.0071020851025,0.));
#14415=CARTESIAN_POINT('Ctrl Pts',(-15.3032539741328,13.0238115816728,0.));
#14416=CARTESIAN_POINT('Ctrl Pts',(-15.3496622219036,13.0402305665115,0.));
#14417=CARTESIAN_POINT('Ctrl Pts',(-15.3962557545684,13.0563577967298,0.));
#14418=CARTESIAN_POINT('Ctrl Pts',(-15.4430330918328,13.0721935806302,0.));
#14419=CARTESIAN_POINT('Ctrl Pts',(-15.4899910401523,13.087740560189,0.));
#14420=CARTESIAN_POINT('Ctrl Pts',(-15.5371254712111,13.1030026646917,0.));
#14421=CARTESIAN_POINT('Ctrl Pts',(-15.5844317820184,13.1179844917497,0.));
#14422=CARTESIAN_POINT('Ctrl Pts',(-15.6319054413079,13.1326905726717,0.));
#14423=CARTESIAN_POINT('Ctrl Pts',(-15.6795425955901,13.147124558532,0.));
#14424=CARTESIAN_POINT('Ctrl Pts',(-15.7273402954914,13.161288914421,0.));
#14425=CARTESIAN_POINT('Ctrl Pts',(-15.7752961549278,13.1751853728467,0.));
#14426=CARTESIAN_POINT('Ctrl Pts',(-15.8234081427091,13.1888152101588,0.));
#14427=CARTESIAN_POINT('Ctrl Pts',(-15.8716743375555,13.2021795724682,0.));
#14428=CARTESIAN_POINT('Ctrl Pts',(-15.9200926550954,13.2152798388134,0.));
#14429=CARTESIAN_POINT('Ctrl Pts',(-15.9686607385389,13.2281177675127,0.));
#14430=CARTESIAN_POINT('Ctrl Pts',(-16.0173761036734,13.240695304984,0.));
#14431=CARTESIAN_POINT('Ctrl Pts',(-16.0662362238032,13.2530144750236,0.));
#14432=CARTESIAN_POINT('Ctrl Pts',(-16.1152386305152,13.2650772466062,0.));
#14433=CARTESIAN_POINT('Ctrl Pts',(-16.1643810242643,13.2768853909882,0.));
#14434=CARTESIAN_POINT('Ctrl Pts',(-16.2136613184475,13.2884404210388,0.));
#14435=CARTESIAN_POINT('Ctrl Pts',(-16.2630775678735,13.2997436744733,0.));
#14436=CARTESIAN_POINT('Ctrl Pts',(-16.3126279218067,13.3107963665229,0.));
#14437=CARTESIAN_POINT('Ctrl Pts',(-16.3623105703343,13.3215996524974,0.));
#14438=CARTESIAN_POINT('Ctrl Pts',(-16.4121236828756,13.3321546976812,0.));
#14439=CARTESIAN_POINT('Ctrl Pts',(-16.4620653818862,13.3424627129921,0.));
#14440=CARTESIAN_POINT('Ctrl Pts',(-16.5121337902953,13.3525249163084,0.));
#14441=CARTESIAN_POINT('Ctrl Pts',(-16.5623270636327,13.3623425108873,0.));
#14442=CARTESIAN_POINT('Ctrl Pts',(-16.612643424234,13.3719166600676,0.));
#14443=CARTESIAN_POINT('Ctrl Pts',(-16.6630812012276,13.381248462113,0.));
#14444=CARTESIAN_POINT('Ctrl Pts',(-16.7136388432444,13.3903389370346,0.));
#14445=CARTESIAN_POINT('Ctrl Pts',(-16.7643148579872,13.3991890464165,0.));
#14446=CARTESIAN_POINT('Ctrl Pts',(-16.8151077630226,13.4077997088426,0.));
#14447=CARTESIAN_POINT('Ctrl Pts',(-16.8660160353187,13.4161718177499,0.));
#14448=CARTESIAN_POINT('Ctrl Pts',(-16.9170380509036,13.4243062623592,0.));
#14449=CARTESIAN_POINT('Ctrl Pts',(-16.9681720567298,13.432203941793,0.));
#14450=CARTESIAN_POINT('Ctrl Pts',(-17.0194162803447,13.4398657451291,0.));
#14451=CARTESIAN_POINT('Ctrl Pts',(-17.0707690194411,13.4472925380889,0.));
#14452=CARTESIAN_POINT('Ctrl Pts',(-17.1222287365697,13.4544851484583,0.));
#14453=CARTESIAN_POINT('Ctrl Pts',(-17.1737941556239,13.4614443545811,0.));
#14454=CARTESIAN_POINT('Ctrl Pts',(-17.235798381426,13.4695161752401,0.));
#14455=CARTESIAN_POINT('Ctrl Pts',(-17.287598725272,13.4759526005425,0.));
#14456=CARTESIAN_POINT('Ctrl Pts',(-17.3291218739796,13.4809165957478,0.));
#14457=CARTESIAN_POINT('Ctrl Pts',(-17.360310805254,13.4845355519784,0.));
#14458=CARTESIAN_POINT('Ctrl Pts',(-17.3811241238545,13.4869019493419,0.));
#14459=CARTESIAN_POINT('Ctrl Pts',(-14.1074595503134,12.4172651441477,13.));
#14460=CARTESIAN_POINT('Ctrl Pts',(-14.1193844248164,12.4277613166149,13.));
#14461=CARTESIAN_POINT('Ctrl Pts',(-14.1315753314249,12.4379186757848,13.));
#14462=CARTESIAN_POINT('Ctrl Pts',(-14.14401474732,12.4477599775084,13.));
#14463=CARTESIAN_POINT('Ctrl Pts',(-14.1585946731696,12.45929471922,13.));
#14464=CARTESIAN_POINT('Ctrl Pts',(-14.1735154808295,12.4703959522577,13.));
#14465=CARTESIAN_POINT('Ctrl Pts',(-14.1887053040703,12.4811568677436,13.));
#14466=CARTESIAN_POINT('Ctrl Pts',(-14.2100781123335,12.4962979908344,13.));
#14467=CARTESIAN_POINT('Ctrl Pts',(-14.2319791941756,12.5107710847127,13.));
#14468=CARTESIAN_POINT('Ctrl Pts',(-14.254157574695,12.5249003586941,13.));
#14469=CARTESIAN_POINT('Ctrl Pts',(-14.2689096955178,12.5342985542355,13.));
#14470=CARTESIAN_POINT('Ctrl Pts',(-14.2837832480516,12.5435462296413,13.));
#14471=CARTESIAN_POINT('Ctrl Pts',(-14.298722508524,12.5527146050322,13.));
#14472=CARTESIAN_POINT('Ctrl Pts',(-14.3144485290642,12.5623658230416,13.));
#14473=CARTESIAN_POINT('Ctrl Pts',(-14.330246820686,12.5719298675028,13.));
#14474=CARTESIAN_POINT('Ctrl Pts',(-14.3460912752807,12.5814385821519,13.));
#14475=CARTESIAN_POINT('Ctrl Pts',(-14.3636874094394,12.5919985302804,13.));
#14476=CARTESIAN_POINT('Ctrl Pts',(-14.381341260665,12.6024891912727,13.));
#14477=CARTESIAN_POINT('Ctrl Pts',(-14.3990589912032,12.6128991700701,13.));
#14478=CARTESIAN_POINT('Ctrl Pts',(-14.4257693299403,12.6285927183677,13.));
#14479=CARTESIAN_POINT('Ctrl Pts',(-14.452628589856,12.6440977931351,13.));
#14480=CARTESIAN_POINT('Ctrl Pts',(-14.4797266308813,12.6592867998067,13.));
#14481=CARTESIAN_POINT('Ctrl Pts',(-14.4994127652612,12.6703212810873,13.));
#14482=CARTESIAN_POINT('Ctrl Pts',(-14.5192269386383,12.6811863451307,13.));
#14483=CARTESIAN_POINT('Ctrl Pts',(-14.5391805041508,12.6918647171384,13.));
#14484=CARTESIAN_POINT('Ctrl Pts',(-14.5635720293892,12.7049181125412,13.));
#14485=CARTESIAN_POINT('Ctrl Pts',(-14.5881710816651,12.7176935524276,13.));
#14486=CARTESIAN_POINT('Ctrl Pts',(-14.612947560673,12.7302281821981,13.));
#14487=CARTESIAN_POINT('Ctrl Pts',(-14.6397102700639,12.7437676626773,13.));
#14488=CARTESIAN_POINT('Ctrl Pts',(-14.6666764215902,12.7570309720221,13.));
#14489=CARTESIAN_POINT('Ctrl Pts',(-14.6937895363403,12.7700903554915,13.));
#14490=CARTESIAN_POINT('Ctrl Pts',(-14.7188202365146,12.7821467169645,13.));
#14491=CARTESIAN_POINT('Ctrl Pts',(-14.7439746960234,12.7940312932614,13.));
#14492=CARTESIAN_POINT('Ctrl Pts',(-14.7692347187417,12.8057660290113,13.));
#14493=CARTESIAN_POINT('Ctrl Pts',(-14.803551756556,12.8217082700361,13.));
#14494=CARTESIAN_POINT('Ctrl Pts',(-14.8380647951195,12.8373723698026,13.));
#14495=CARTESIAN_POINT('Ctrl Pts',(-14.8727890594695,12.8527323828632,13.));
#14496=CARTESIAN_POINT('Ctrl Pts',(-14.9062972246235,12.8675544637349,13.));
#14497=CARTESIAN_POINT('Ctrl Pts',(-14.9400067536049,12.8820871276608,13.));
#14498=CARTESIAN_POINT('Ctrl Pts',(-14.9739251233868,12.8963159096104,13.));
#14499=CARTESIAN_POINT('Ctrl Pts',(-15.0200041787641,12.9156461084266,13.));
#14500=CARTESIAN_POINT('Ctrl Pts',(-15.0664667162746,12.9344180544673,13.));
#14501=CARTESIAN_POINT('Ctrl Pts',(-15.1132567586771,12.9526968521306,13.));
#14502=CARTESIAN_POINT('Ctrl Pts',(-15.1543841890161,12.968763518006,13.));
#14503=CARTESIAN_POINT('Ctrl Pts',(-15.195760575808,12.9844546719519,13.));
#14504=CARTESIAN_POINT('Ctrl Pts',(-15.2373637638391,12.9997938464524,13.));
#14505=CARTESIAN_POINT('Ctrl Pts',(-15.298696963875,13.0224075138791,13.));
#14506=CARTESIAN_POINT('Ctrl Pts',(-15.3605284720727,13.0442489122199,13.));
#14507=CARTESIAN_POINT('Ctrl Pts',(-15.4228468913963,13.0653151028182,13.));
#14508=CARTESIAN_POINT('Ctrl Pts',(-15.501493344391,13.0919008408175,13.));
#14509=CARTESIAN_POINT('Ctrl Pts',(-15.580912148319,13.1172560779889,13.));
#14510=CARTESIAN_POINT('Ctrl Pts',(-15.6610132193903,13.1414683121723,13.));
#14511=CARTESIAN_POINT('Ctrl Pts',(-15.7695162957074,13.1742656500639,13.));
#14512=CARTESIAN_POINT('Ctrl Pts',(-15.8792747460898,13.2049609859192,13.));
#14513=CARTESIAN_POINT('Ctrl Pts',(-15.9901726544041,13.2336341230354,13.));
#14514=CARTESIAN_POINT('Ctrl Pts',(-16.089041043312,13.2591969755247,13.));
#14515=CARTESIAN_POINT('Ctrl Pts',(-16.1888100042035,13.2831593506295,13.));
#14516=CARTESIAN_POINT('Ctrl Pts',(-16.2893994149303,13.305579935219,13.));
#14517=CARTESIAN_POINT('Ctrl Pts',(-16.4319622721867,13.3373560692807,13.));
#14518=CARTESIAN_POINT('Ctrl Pts',(-16.5761757269041,13.3660302366011,13.));
#14519=CARTESIAN_POINT('Ctrl Pts',(-16.7218506225541,13.3917254924233,13.));
#14520=CARTESIAN_POINT('Ctrl Pts',(-16.8350074321741,13.4116849587284,13.));
#14521=CARTESIAN_POINT('Ctrl Pts',(-16.9490507104974,13.4298451938425,13.));
#14522=CARTESIAN_POINT('Ctrl Pts',(-17.063896781128,13.4462507334689,13.));
#14523=CARTESIAN_POINT('Ctrl Pts',(-17.1632473211086,13.4604427664362,13.));
#14524=CARTESIAN_POINT('Ctrl Pts',(-17.2631945741556,13.4733230167208,13.));
#14525=CARTESIAN_POINT('Ctrl Pts',(-17.363718437608,13.4849093843288,13.));
#14526=CARTESIAN_POINT('Ctrl Pts',(-17.3695184016672,13.4855778874423,13.));
#14527=CARTESIAN_POINT('Ctrl Pts',(-17.3753202971203,13.4862420757008,13.));
#14528=CARTESIAN_POINT('Ctrl Pts',(-17.3811241238545,13.4869019493419,13.));
#14529=CARTESIAN_POINT('Ctrl Pts',(-13.4869019493419,17.3811241238545,0.));
#14530=CARTESIAN_POINT('Ctrl Pts',(-13.4869019493419,17.3811241238545,21.));
#14531=CARTESIAN_POINT('Ctrl Pts',(-13.485718750657,17.3707174645609,0.));
#14532=CARTESIAN_POINT('Ctrl Pts',(-13.485718750657,17.3707174645609,21.));
#14533=CARTESIAN_POINT('Ctrl Pts',(-13.4833292332349,17.3499144948292,0.));
#14534=CARTESIAN_POINT('Ctrl Pts',(-13.4833292332349,17.3499144948292,21.));
#14535=CARTESIAN_POINT('Ctrl Pts',(-13.4796755969465,17.3187410868027,0.));
#14536=CARTESIAN_POINT('Ctrl Pts',(-13.4796755969465,17.3187410868027,21.));
#14537=CARTESIAN_POINT('Ctrl Pts',(-13.474665315482,17.2772386565028,0.));
#14538=CARTESIAN_POINT('Ctrl Pts',(-13.474665315482,17.2772386565028,21.));
#14539=CARTESIAN_POINT('Ctrl Pts',(-13.4681708717969,17.2254643437923,0.));
#14540=CARTESIAN_POINT('Ctrl Pts',(-13.4681708717969,17.2254643437923,21.));
#14541=CARTESIAN_POINT('Ctrl Pts',(-13.4614443545811,17.173794155624,0.));
#14542=CARTESIAN_POINT('Ctrl Pts',(-13.4614443545811,17.173794155624,21.));
#14543=CARTESIAN_POINT('Ctrl Pts',(-13.4544851484583,17.1222287365697,0.));
#14544=CARTESIAN_POINT('Ctrl Pts',(-13.4544851484583,17.1222287365697,21.));
#14545=CARTESIAN_POINT('Ctrl Pts',(-13.4472925380889,17.0707690194412,0.));
#14546=CARTESIAN_POINT('Ctrl Pts',(-13.4472925380889,17.0707690194412,21.));
#14547=CARTESIAN_POINT('Ctrl Pts',(-13.4398657451291,17.0194162803447,0.));
#14548=CARTESIAN_POINT('Ctrl Pts',(-13.4398657451291,17.0194162803447,21.));
#14549=CARTESIAN_POINT('Ctrl Pts',(-13.432203941793,16.9681720567298,0.));
#14550=CARTESIAN_POINT('Ctrl Pts',(-13.432203941793,16.9681720567298,21.));
#14551=CARTESIAN_POINT('Ctrl Pts',(-13.4243062623592,16.9170380509036,0.));
#14552=CARTESIAN_POINT('Ctrl Pts',(-13.4243062623592,16.9170380509036,21.));
#14553=CARTESIAN_POINT('Ctrl Pts',(-13.4161718177499,16.8660160353187,0.));
#14554=CARTESIAN_POINT('Ctrl Pts',(-13.4161718177499,16.8660160353187,21.));
#14555=CARTESIAN_POINT('Ctrl Pts',(-13.4077997088426,16.8151077630226,0.));
#14556=CARTESIAN_POINT('Ctrl Pts',(-13.4077997088426,16.8151077630226,21.));
#14557=CARTESIAN_POINT('Ctrl Pts',(-13.3991890464165,16.7643148579873,0.));
#14558=CARTESIAN_POINT('Ctrl Pts',(-13.3991890464165,16.7643148579873,21.));
#14559=CARTESIAN_POINT('Ctrl Pts',(-13.3903389370346,16.7136388432444,0.));
#14560=CARTESIAN_POINT('Ctrl Pts',(-13.3903389370346,16.7136388432444,21.));
#14561=CARTESIAN_POINT('Ctrl Pts',(-13.381248462113,16.6630812012276,0.));
#14562=CARTESIAN_POINT('Ctrl Pts',(-13.381248462113,16.6630812012276,21.));
#14563=CARTESIAN_POINT('Ctrl Pts',(-13.3719166600676,16.612643424234,0.));
#14564=CARTESIAN_POINT('Ctrl Pts',(-13.3719166600676,16.612643424234,21.));
#14565=CARTESIAN_POINT('Ctrl Pts',(-13.3623425108873,16.5623270636327,0.));
#14566=CARTESIAN_POINT('Ctrl Pts',(-13.3623425108873,16.5623270636327,21.));
#14567=CARTESIAN_POINT('Ctrl Pts',(-13.3525249163084,16.5121337902953,0.));
#14568=CARTESIAN_POINT('Ctrl Pts',(-13.3525249163084,16.5121337902953,21.));
#14569=CARTESIAN_POINT('Ctrl Pts',(-13.3424627129921,16.4620653818862,0.));
#14570=CARTESIAN_POINT('Ctrl Pts',(-13.3424627129921,16.4620653818862,21.));
#14571=CARTESIAN_POINT('Ctrl Pts',(-13.3321546976812,16.4121236828756,0.));
#14572=CARTESIAN_POINT('Ctrl Pts',(-13.3321546976812,16.4121236828756,21.));
#14573=CARTESIAN_POINT('Ctrl Pts',(-13.3215996524974,16.3623105703343,0.));
#14574=CARTESIAN_POINT('Ctrl Pts',(-13.3215996524974,16.3623105703343,21.));
#14575=CARTESIAN_POINT('Ctrl Pts',(-13.3107963665229,16.3126279218067,0.));
#14576=CARTESIAN_POINT('Ctrl Pts',(-13.3107963665229,16.3126279218067,21.));
#14577=CARTESIAN_POINT('Ctrl Pts',(-13.2997436744733,16.2630775678735,0.));
#14578=CARTESIAN_POINT('Ctrl Pts',(-13.2997436744733,16.2630775678735,21.));
#14579=CARTESIAN_POINT('Ctrl Pts',(-13.2884404210387,16.2136613184475,0.));
#14580=CARTESIAN_POINT('Ctrl Pts',(-13.2884404210387,16.2136613184475,21.));
#14581=CARTESIAN_POINT('Ctrl Pts',(-13.2768853909882,16.1643810242643,0.));
#14582=CARTESIAN_POINT('Ctrl Pts',(-13.2768853909882,16.1643810242643,21.));
#14583=CARTESIAN_POINT('Ctrl Pts',(-13.2650772466062,16.1152386305152,0.));
#14584=CARTESIAN_POINT('Ctrl Pts',(-13.2650772466062,16.1152386305152,21.));
#14585=CARTESIAN_POINT('Ctrl Pts',(-13.2530144750236,16.0662362238032,0.));
#14586=CARTESIAN_POINT('Ctrl Pts',(-13.2530144750236,16.0662362238032,21.));
#14587=CARTESIAN_POINT('Ctrl Pts',(-13.240695304984,16.0173761036734,0.));
#14588=CARTESIAN_POINT('Ctrl Pts',(-13.240695304984,16.0173761036734,21.));
#14589=CARTESIAN_POINT('Ctrl Pts',(-13.2281177675127,15.9686607385389,0.));
#14590=CARTESIAN_POINT('Ctrl Pts',(-13.2281177675127,15.9686607385389,21.));
#14591=CARTESIAN_POINT('Ctrl Pts',(-13.2152798388134,15.9200926550954,0.));
#14592=CARTESIAN_POINT('Ctrl Pts',(-13.2152798388134,15.9200926550954,21.));
#14593=CARTESIAN_POINT('Ctrl Pts',(-13.2021795724682,15.8716743375555,0.));
#14594=CARTESIAN_POINT('Ctrl Pts',(-13.2021795724682,15.8716743375555,21.));
#14595=CARTESIAN_POINT('Ctrl Pts',(-13.1888152101588,15.8234081427091,0.));
#14596=CARTESIAN_POINT('Ctrl Pts',(-13.1888152101588,15.8234081427091,21.));
#14597=CARTESIAN_POINT('Ctrl Pts',(-13.1751853728467,15.7752961549278,0.));
#14598=CARTESIAN_POINT('Ctrl Pts',(-13.1751853728467,15.7752961549278,21.));
#14599=CARTESIAN_POINT('Ctrl Pts',(-13.161288914421,15.7273402954914,0.));
#14600=CARTESIAN_POINT('Ctrl Pts',(-13.161288914421,15.7273402954914,21.));
#14601=CARTESIAN_POINT('Ctrl Pts',(-13.147124558532,15.6795425955901,0.));
#14602=CARTESIAN_POINT('Ctrl Pts',(-13.147124558532,15.6795425955901,21.));
#14603=CARTESIAN_POINT('Ctrl Pts',(-13.1326905726717,15.6319054413079,0.));
#14604=CARTESIAN_POINT('Ctrl Pts',(-13.1326905726717,15.6319054413079,21.));
#14605=CARTESIAN_POINT('Ctrl Pts',(-13.1179844917497,15.5844317820184,0.));
#14606=CARTESIAN_POINT('Ctrl Pts',(-13.1179844917497,15.5844317820184,21.));
#14607=CARTESIAN_POINT('Ctrl Pts',(-13.1030026646917,15.5371254712111,0.));
#14608=CARTESIAN_POINT('Ctrl Pts',(-13.1030026646917,15.5371254712111,21.));
#14609=CARTESIAN_POINT('Ctrl Pts',(-13.087740560189,15.4899910401523,0.));
#14610=CARTESIAN_POINT('Ctrl Pts',(-13.087740560189,15.4899910401523,21.));
#14611=CARTESIAN_POINT('Ctrl Pts',(-13.0721935806302,15.4430330918328,0.));
#14612=CARTESIAN_POINT('Ctrl Pts',(-13.0721935806302,15.4430330918328,21.));
#14613=CARTESIAN_POINT('Ctrl Pts',(-13.0563577967298,15.3962557545684,0.));
#14614=CARTESIAN_POINT('Ctrl Pts',(-13.0563577967298,15.3962557545684,21.));
#14615=CARTESIAN_POINT('Ctrl Pts',(-13.0402305665115,15.3496622219036,0.));
#14616=CARTESIAN_POINT('Ctrl Pts',(-13.0402305665115,15.3496622219036,21.));
#14617=CARTESIAN_POINT('Ctrl Pts',(-13.0238115816728,15.3032539741328,0.));
#14618=CARTESIAN_POINT('Ctrl Pts',(-13.0238115816728,15.3032539741328,21.));
#14619=CARTESIAN_POINT('Ctrl Pts',(-13.0071020851025,15.2570313635503,0.));
#14620=CARTESIAN_POINT('Ctrl Pts',(-13.0071020851025,15.2570313635503,21.));
#14621=CARTESIAN_POINT('Ctrl Pts',(-12.9901029059182,15.2109950816083,0.));
#14622=CARTESIAN_POINT('Ctrl Pts',(-12.9901029059182,15.2109950816083,21.));
#14623=CARTESIAN_POINT('Ctrl Pts',(-12.9728126886697,15.1651474813659,0.));
#14624=CARTESIAN_POINT('Ctrl Pts',(-12.9728126886697,15.1651474813659,21.));
#14625=CARTESIAN_POINT('Ctrl Pts',(-12.9552263908864,15.1194937003528,0.));
#14626=CARTESIAN_POINT('Ctrl Pts',(-12.9552263908864,15.1194937003528,21.));
#14627=CARTESIAN_POINT('Ctrl Pts',(-12.9373327960422,15.0740435169624,0.));
#14628=CARTESIAN_POINT('Ctrl Pts',(-12.9373327960422,15.0740435169624,21.));
#14629=CARTESIAN_POINT('Ctrl Pts',(-12.9191164383568,15.0288099208306,0.));
#14630=CARTESIAN_POINT('Ctrl Pts',(-12.9191164383568,15.0288099208306,21.));
#14631=CARTESIAN_POINT('Ctrl Pts',(-12.9005620742036,14.9838057866976,0.));
#14632=CARTESIAN_POINT('Ctrl Pts',(-12.9005620742036,14.9838057866976,21.));
#14633=CARTESIAN_POINT('Ctrl Pts',(-12.8816587472147,14.9390408507356,0.));
#14634=CARTESIAN_POINT('Ctrl Pts',(-12.8816587472147,14.9390408507356,21.));
#14635=CARTESIAN_POINT('Ctrl Pts',(-12.8624032236317,14.8945191569251,0.));
#14636=CARTESIAN_POINT('Ctrl Pts',(-12.8624032236317,14.8945191569251,21.));
#14637=CARTESIAN_POINT('Ctrl Pts',(-12.8428057266944,14.8502347891476,0.));
#14638=CARTESIAN_POINT('Ctrl Pts',(-12.8428057266944,14.8502347891476,21.));
#14639=CARTESIAN_POINT('Ctrl Pts',(-12.8228846016791,14.8061758577898,0.));
#14640=CARTESIAN_POINT('Ctrl Pts',(-12.8228846016791,14.8061758577898,21.));
#14641=CARTESIAN_POINT('Ctrl Pts',(-12.8026557145457,14.7623324139791,0.));
#14642=CARTESIAN_POINT('Ctrl Pts',(-12.8026557145457,14.7623324139791,21.));
#14643=CARTESIAN_POINT('Ctrl Pts',(-12.7821227233337,14.7187037124277,0.));
#14644=CARTESIAN_POINT('Ctrl Pts',(-12.7821227233337,14.7187037124277,21.));
#14645=CARTESIAN_POINT('Ctrl Pts',(-12.7612687078867,14.6753044633399,0.));
#14646=CARTESIAN_POINT('Ctrl Pts',(-12.7612687078867,14.6753044633399,21.));
#14647=CARTESIAN_POINT('Ctrl Pts',(-12.7400427996251,14.6321748083434,0.));
#14648=CARTESIAN_POINT('Ctrl Pts',(-12.7400427996251,14.6321748083434,21.));
#14649=CARTESIAN_POINT('Ctrl Pts',(-12.7183743139638,14.5893698147583,0.));
#14650=CARTESIAN_POINT('Ctrl Pts',(-12.7183743139638,14.5893698147583,21.));
#14651=CARTESIAN_POINT('Ctrl Pts',(-12.6961966430455,14.5469417071952,0.));
#14652=CARTESIAN_POINT('Ctrl Pts',(-12.6961966430455,14.5469417071952,21.));
#14653=CARTESIAN_POINT('Ctrl Pts',(-12.6734695081852,14.5049233087958,0.));
#14654=CARTESIAN_POINT('Ctrl Pts',(-12.6734695081852,14.5049233087958,21.));
#14655=CARTESIAN_POINT('Ctrl Pts',(-12.6501984687124,14.463313553928,0.));
#14656=CARTESIAN_POINT('Ctrl Pts',(-12.6501984687124,14.463313553928,21.));
#14657=CARTESIAN_POINT('Ctrl Pts',(-12.626464614311,14.4220553460485,0.));
#14658=CARTESIAN_POINT('Ctrl Pts',(-12.626464614311,14.4220553460485,21.));
#14659=CARTESIAN_POINT('Ctrl Pts',(-12.6023830189244,14.3810669346235,0.));
#14660=CARTESIAN_POINT('Ctrl Pts',(-12.6023830189244,14.3810669346235,21.));
#14661=CARTESIAN_POINT('Ctrl Pts',(-12.5780443898087,14.3402859058353,0.));
#14662=CARTESIAN_POINT('Ctrl Pts',(-12.5780443898087,14.3402859058353,21.));
#14663=CARTESIAN_POINT('Ctrl Pts',(-12.5534605602317,14.2997103098726,0.));
#14664=CARTESIAN_POINT('Ctrl Pts',(-12.5534605602317,14.2997103098726,21.));
#14665=CARTESIAN_POINT('Ctrl Pts',(-12.5285125321527,14.2594378207584,0.));
#14666=CARTESIAN_POINT('Ctrl Pts',(-12.5285125321527,14.2594378207584,21.));
#14667=CARTESIAN_POINT('Ctrl Pts',(-12.502885965175,14.2197144660135,0.));
#14668=CARTESIAN_POINT('Ctrl Pts',(-12.502885965175,14.2197144660135,21.));
#14669=CARTESIAN_POINT('Ctrl Pts',(-12.4761570639125,14.1808688343892,0.));
#14670=CARTESIAN_POINT('Ctrl Pts',(-12.4761570639125,14.1808688343892,21.));
#14671=CARTESIAN_POINT('Ctrl Pts',(-12.4535485619996,14.1507598477672,0.));
#14672=CARTESIAN_POINT('Ctrl Pts',(-12.4535485619996,14.1507598477672,21.));
#14673=CARTESIAN_POINT('Ctrl Pts',(-12.4357509724316,14.1288394445866,0.));
#14674=CARTESIAN_POINT('Ctrl Pts',(-12.4357509724316,14.1288394445866,21.));
#14675=CARTESIAN_POINT('Ctrl Pts',(-12.4234926340671,14.1145347042316,0.));
#14676=CARTESIAN_POINT('Ctrl Pts',(-12.4234926340671,14.1145347042316,21.));
#14677=CARTESIAN_POINT('Ctrl Pts',(-12.4172651441477,14.1074595503134,0.));
#14678=CARTESIAN_POINT('Ctrl Pts',(-12.4172651441477,14.1074595503134,21.));
#14679=CARTESIAN_POINT('',(-13.486901949342,17.3811241238545,0.));
#14680=CARTESIAN_POINT('Ctrl Pts',(-12.4172651441477,14.1074595503134,0.));
#14681=CARTESIAN_POINT('Ctrl Pts',(-12.4234926340671,14.1145347042316,0.));
#14682=CARTESIAN_POINT('Ctrl Pts',(-12.4357509724316,14.1288394445866,0.));
#14683=CARTESIAN_POINT('Ctrl Pts',(-12.4535485619996,14.1507598477672,0.));
#14684=CARTESIAN_POINT('Ctrl Pts',(-12.4761570639125,14.1808688343892,0.));
#14685=CARTESIAN_POINT('Ctrl Pts',(-12.502885965175,14.2197144660135,0.));
#14686=CARTESIAN_POINT('Ctrl Pts',(-12.5285125321527,14.2594378207584,0.));
#14687=CARTESIAN_POINT('Ctrl Pts',(-12.5534605602317,14.2997103098726,0.));
#14688=CARTESIAN_POINT('Ctrl Pts',(-12.5780443898087,14.3402859058353,0.));
#14689=CARTESIAN_POINT('Ctrl Pts',(-12.6023830189244,14.3810669346235,0.));
#14690=CARTESIAN_POINT('Ctrl Pts',(-12.626464614311,14.4220553460485,0.));
#14691=CARTESIAN_POINT('Ctrl Pts',(-12.6501984687124,14.463313553928,0.));
#14692=CARTESIAN_POINT('Ctrl Pts',(-12.6734695081852,14.5049233087958,0.));
#14693=CARTESIAN_POINT('Ctrl Pts',(-12.6961966430455,14.5469417071952,0.));
#14694=CARTESIAN_POINT('Ctrl Pts',(-12.7183743139638,14.5893698147583,0.));
#14695=CARTESIAN_POINT('Ctrl Pts',(-12.7400427996251,14.6321748083434,0.));
#14696=CARTESIAN_POINT('Ctrl Pts',(-12.7612687078867,14.6753044633399,0.));
#14697=CARTESIAN_POINT('Ctrl Pts',(-12.7821227233337,14.7187037124277,0.));
#14698=CARTESIAN_POINT('Ctrl Pts',(-12.8026557145457,14.7623324139791,0.));
#14699=CARTESIAN_POINT('Ctrl Pts',(-12.8228846016791,14.8061758577898,0.));
#14700=CARTESIAN_POINT('Ctrl Pts',(-12.8428057266944,14.8502347891476,0.));
#14701=CARTESIAN_POINT('Ctrl Pts',(-12.8624032236317,14.8945191569251,0.));
#14702=CARTESIAN_POINT('Ctrl Pts',(-12.8816587472147,14.9390408507356,0.));
#14703=CARTESIAN_POINT('Ctrl Pts',(-12.9005620742036,14.9838057866976,0.));
#14704=CARTESIAN_POINT('Ctrl Pts',(-12.9191164383568,15.0288099208306,0.));
#14705=CARTESIAN_POINT('Ctrl Pts',(-12.9373327960422,15.0740435169624,0.));
#14706=CARTESIAN_POINT('Ctrl Pts',(-12.9552263908864,15.1194937003528,0.));
#14707=CARTESIAN_POINT('Ctrl Pts',(-12.9728126886697,15.1651474813659,0.));
#14708=CARTESIAN_POINT('Ctrl Pts',(-12.9901029059182,15.2109950816083,0.));
#14709=CARTESIAN_POINT('Ctrl Pts',(-13.0071020851025,15.2570313635503,0.));
#14710=CARTESIAN_POINT('Ctrl Pts',(-13.0238115816728,15.3032539741328,0.));
#14711=CARTESIAN_POINT('Ctrl Pts',(-13.0402305665115,15.3496622219036,0.));
#14712=CARTESIAN_POINT('Ctrl Pts',(-13.0563577967298,15.3962557545684,0.));
#14713=CARTESIAN_POINT('Ctrl Pts',(-13.0721935806302,15.4430330918328,0.));
#14714=CARTESIAN_POINT('Ctrl Pts',(-13.087740560189,15.4899910401523,0.));
#14715=CARTESIAN_POINT('Ctrl Pts',(-13.1030026646917,15.5371254712111,0.));
#14716=CARTESIAN_POINT('Ctrl Pts',(-13.1179844917497,15.5844317820184,0.));
#14717=CARTESIAN_POINT('Ctrl Pts',(-13.1326905726717,15.6319054413079,0.));
#14718=CARTESIAN_POINT('Ctrl Pts',(-13.147124558532,15.6795425955901,0.));
#14719=CARTESIAN_POINT('Ctrl Pts',(-13.161288914421,15.7273402954914,0.));
#14720=CARTESIAN_POINT('Ctrl Pts',(-13.1751853728467,15.7752961549278,0.));
#14721=CARTESIAN_POINT('Ctrl Pts',(-13.1888152101588,15.8234081427091,0.));
#14722=CARTESIAN_POINT('Ctrl Pts',(-13.2021795724682,15.8716743375555,0.));
#14723=CARTESIAN_POINT('Ctrl Pts',(-13.2152798388134,15.9200926550954,0.));
#14724=CARTESIAN_POINT('Ctrl Pts',(-13.2281177675127,15.9686607385389,0.));
#14725=CARTESIAN_POINT('Ctrl Pts',(-13.240695304984,16.0173761036734,0.));
#14726=CARTESIAN_POINT('Ctrl Pts',(-13.2530144750236,16.0662362238032,0.));
#14727=CARTESIAN_POINT('Ctrl Pts',(-13.2650772466062,16.1152386305152,0.));
#14728=CARTESIAN_POINT('Ctrl Pts',(-13.2768853909882,16.1643810242643,0.));
#14729=CARTESIAN_POINT('Ctrl Pts',(-13.2884404210387,16.2136613184475,0.));
#14730=CARTESIAN_POINT('Ctrl Pts',(-13.2997436744733,16.2630775678735,0.));
#14731=CARTESIAN_POINT('Ctrl Pts',(-13.3107963665229,16.3126279218067,0.));
#14732=CARTESIAN_POINT('Ctrl Pts',(-13.3215996524974,16.3623105703343,0.));
#14733=CARTESIAN_POINT('Ctrl Pts',(-13.3321546976812,16.4121236828756,0.));
#14734=CARTESIAN_POINT('Ctrl Pts',(-13.3424627129921,16.4620653818862,0.));
#14735=CARTESIAN_POINT('Ctrl Pts',(-13.3525249163084,16.5121337902953,0.));
#14736=CARTESIAN_POINT('Ctrl Pts',(-13.3623425108873,16.5623270636327,0.));
#14737=CARTESIAN_POINT('Ctrl Pts',(-13.3719166600676,16.612643424234,0.));
#14738=CARTESIAN_POINT('Ctrl Pts',(-13.381248462113,16.6630812012276,0.));
#14739=CARTESIAN_POINT('Ctrl Pts',(-13.3903389370346,16.7136388432444,0.));
#14740=CARTESIAN_POINT('Ctrl Pts',(-13.3991890464165,16.7643148579873,0.));
#14741=CARTESIAN_POINT('Ctrl Pts',(-13.4077997088426,16.8151077630226,0.));
#14742=CARTESIAN_POINT('Ctrl Pts',(-13.4161718177499,16.8660160353187,0.));
#14743=CARTESIAN_POINT('Ctrl Pts',(-13.4243062623592,16.9170380509036,0.));
#14744=CARTESIAN_POINT('Ctrl Pts',(-13.432203941793,16.9681720567298,0.));
#14745=CARTESIAN_POINT('Ctrl Pts',(-13.4398657451291,17.0194162803447,0.));
#14746=CARTESIAN_POINT('Ctrl Pts',(-13.4472925380889,17.0707690194412,0.));
#14747=CARTESIAN_POINT('Ctrl Pts',(-13.4544851484583,17.1222287365697,0.));
#14748=CARTESIAN_POINT('Ctrl Pts',(-13.4614443545811,17.173794155624,0.));
#14749=CARTESIAN_POINT('Ctrl Pts',(-13.4695161752401,17.235798381426,0.));
#14750=CARTESIAN_POINT('Ctrl Pts',(-13.4759526005425,17.287598725272,0.));
#14751=CARTESIAN_POINT('Ctrl Pts',(-13.4809165957478,17.3291218739796,0.));
#14752=CARTESIAN_POINT('Ctrl Pts',(-13.4845355519784,17.360310805254,0.));
#14753=CARTESIAN_POINT('Ctrl Pts',(-13.4869019493419,17.3811241238545,0.));
#14754=CARTESIAN_POINT('',(-13.486901949342,17.3811241238545,13.));
#14755=CARTESIAN_POINT('Ctrl Pts',(-13.4869019493419,17.3811241238545,13.));
#14756=CARTESIAN_POINT('Ctrl Pts',(-13.475253226354,17.2786694026925,13.));
#14757=CARTESIAN_POINT('Ctrl Pts',(-13.4622625504827,17.1768129075703,13.));
#14758=CARTESIAN_POINT('Ctrl Pts',(-13.4479123002588,17.0755735571127,13.));
#14759=CARTESIAN_POINT('Ctrl Pts',(-13.4241333152838,16.9078155768783,13.));
#14760=CARTESIAN_POINT('Ctrl Pts',(-13.3966181281356,16.7417653304334,13.));
#14761=CARTESIAN_POINT('Ctrl Pts',(-13.365224404591,16.57767452627,13.));
#14762=CARTESIAN_POINT('Ctrl Pts',(-13.341093348038,16.4515447134285,13.));
#14763=CARTESIAN_POINT('Ctrl Pts',(-13.3146689195875,16.3265706105421,13.));
#14764=CARTESIAN_POINT('Ctrl Pts',(-13.2858665160047,16.2028831155019,13.));
#14765=CARTESIAN_POINT('Ctrl Pts',(-13.2548614253288,16.06973651931,13.));
#14766=CARTESIAN_POINT('Ctrl Pts',(-13.221105276728,15.9380763844413,13.));
#14767=CARTESIAN_POINT('Ctrl Pts',(-13.1844379732027,15.8081115249869,13.));
#14768=CARTESIAN_POINT('Ctrl Pts',(-13.1641379552808,15.7361594390004,13.));
#14769=CARTESIAN_POINT('Ctrl Pts',(-13.1429498666824,15.6647240119351,13.));
#14770=CARTESIAN_POINT('Ctrl Pts',(-13.1208442193483,15.5938437094451,13.));
#14771=CARTESIAN_POINT('Ctrl Pts',(-13.0995423541465,15.5255406814322,13.));
#14772=CARTESIAN_POINT('Ctrl Pts',(-13.0773830005559,15.4577571787665,13.));
#14773=CARTESIAN_POINT('Ctrl Pts',(-13.0543129132427,15.3905488552889,13.));
#14774=CARTESIAN_POINT('Ctrl Pts',(-13.0343732800281,15.33246024466,13.));
#14775=CARTESIAN_POINT('Ctrl Pts',(-13.0137559287927,15.2747993584962,13.));
#14776=CARTESIAN_POINT('Ctrl Pts',(-12.9924643459712,15.2175748374047,13.));
#14777=CARTESIAN_POINT('Ctrl Pts',(-12.9771843404906,15.1765073882052,13.));
#14778=CARTESIAN_POINT('Ctrl Pts',(-12.9615593601525,15.1356630008116,13.));
#14779=CARTESIAN_POINT('Ctrl Pts',(-12.9455599556256,15.0950681407047,13.));
#14780=CARTESIAN_POINT('Ctrl Pts',(-12.9298210808671,15.0551343157937,13.));
#14781=CARTESIAN_POINT('Ctrl Pts',(-12.9137147531571,15.0154457689919,13.));
#14782=CARTESIAN_POINT('Ctrl Pts',(-12.8972012565818,14.9760367892541,13.));
#14783=CARTESIAN_POINT('Ctrl Pts',(-12.8828830850643,14.9418668889764,13.));
#14784=CARTESIAN_POINT('Ctrl Pts',(-12.8682568220943,14.9079086467,13.));
#14785=CARTESIAN_POINT('Ctrl Pts',(-12.853336407922,14.8741550424141,13.));
#14786=CARTESIAN_POINT('Ctrl Pts',(-12.8398219364233,14.8435820222663,13.));
#14787=CARTESIAN_POINT('Ctrl Pts',(-12.8260705988221,14.8131735649528,13.));
#14788=CARTESIAN_POINT('Ctrl Pts',(-12.8121025758909,14.782917409017,13.));
#14789=CARTESIAN_POINT('Ctrl Pts',(-12.8003366510026,14.7574312210357,13.));
#14790=CARTESIAN_POINT('Ctrl Pts',(-12.7884183713523,14.7320520621591,13.));
#14791=CARTESIAN_POINT('Ctrl Pts',(-12.7763327021684,14.7067929859341,13.));
#14792=CARTESIAN_POINT('Ctrl Pts',(-12.7588434232842,14.6702403530813,13.));
#14793=CARTESIAN_POINT('Ctrl Pts',(-12.7410029355977,14.6339396294117,13.));
#14794=CARTESIAN_POINT('Ctrl Pts',(-12.7226389620173,14.5980256539368,13.));
#14795=CARTESIAN_POINT('Ctrl Pts',(-12.7115427372118,14.5763250375761,13.));
#14796=CARTESIAN_POINT('Ctrl Pts',(-12.7002526009286,14.5547677199977,13.));
#14797=CARTESIAN_POINT('Ctrl Pts',(-12.6887481998661,14.533370542697,13.));
#14798=CARTESIAN_POINT('Ctrl Pts',(-12.6781379056319,14.513636325704,13.));
#14799=CARTESIAN_POINT('Ctrl Pts',(-12.6673442954742,14.494039116296,13.));
#14800=CARTESIAN_POINT('Ctrl Pts',(-12.656388173598,14.4745649059699,13.));
#14801=CARTESIAN_POINT('Ctrl Pts',(-12.6413169181342,14.4477761569858,13.));
#14802=CARTESIAN_POINT('Ctrl Pts',(-12.6259439377184,14.4212156950323,13.));
#14803=CARTESIAN_POINT('Ctrl Pts',(-12.610392584142,14.3947967980035,13.));
#14804=CARTESIAN_POINT('Ctrl Pts',(-12.6005265277046,14.3780361779186,13.));
#14805=CARTESIAN_POINT('Ctrl Pts',(-12.5905900370373,14.3613315561545,13.));
#14806=CARTESIAN_POINT('Ctrl Pts',(-12.5805908896179,14.3446791500623,13.));
#14807=CARTESIAN_POINT('Ctrl Pts',(-12.5716171202366,14.3297343907096,13.));
#14808=CARTESIAN_POINT('Ctrl Pts',(-12.5625934694128,14.3148312513707,13.));
#14809=CARTESIAN_POINT('Ctrl Pts',(-12.5534931963782,14.2999916563209,13.));
#14810=CARTESIAN_POINT('Ctrl Pts',(-12.543926997017,14.2843922864836,13.));
#14811=CARTESIAN_POINT('Ctrl Pts',(-12.5342762592095,14.2688630442666,13.));
#14812=CARTESIAN_POINT('Ctrl Pts',(-12.5244602884878,14.2534670740361,13.));
#14813=CARTESIAN_POINT('Ctrl Pts',(-12.5081559827352,14.2278944013872,13.));
#14814=CARTESIAN_POINT('Ctrl Pts',(-12.4913891918921,14.2026946288704,13.));
#14815=CARTESIAN_POINT('Ctrl Pts',(-12.4736648236058,14.1782508275765,13.));
#14816=CARTESIAN_POINT('Ctrl Pts',(-12.4638909761696,14.1647716456531,13.));
#14817=CARTESIAN_POINT('Ctrl Pts',(-12.4538248359232,14.1515231428601,13.));
#14818=CARTESIAN_POINT('Ctrl Pts',(-12.443405435509,14.1385523184119,13.));
#14819=CARTESIAN_POINT('Ctrl Pts',(-12.4349297906026,14.1280012216313,13.));
#14820=CARTESIAN_POINT('Ctrl Pts',(-12.4262204477521,14.1176338183099,13.));
#14821=CARTESIAN_POINT('Ctrl Pts',(-12.4172651441477,14.1074595503134,13.));
#14822=CARTESIAN_POINT('',(-13.486901949342,17.3811241238545,0.));
#14823=CARTESIAN_POINT('Origin',(-3.33073116609659E-12,4.58435815896522E-12,
0.));
#14824=CARTESIAN_POINT('',(-12.3627494547115,18.1978687191668,0.));
#14825=CARTESIAN_POINT('Origin',(-3.33073116609659E-12,4.58435815896522E-12,
0.));
#14826=CARTESIAN_POINT('',(-12.3627494547115,18.1978687191668,13.));
#14827=CARTESIAN_POINT('Origin',(-3.33073116609659E-12,4.58435815896522E-12,
13.));
#14828=CARTESIAN_POINT('',(-12.3627494547115,18.1978687191668,0.));
#14829=CARTESIAN_POINT('Ctrl Pts',(-9.57984538049455,16.1689656784104,0.));
#14830=CARTESIAN_POINT('Ctrl Pts',(-9.57984538049455,16.1689656784104,21.));
#14831=CARTESIAN_POINT('Ctrl Pts',(-9.58464985151482,16.1770747160769,0.));
#14832=CARTESIAN_POINT('Ctrl Pts',(-9.58464985151482,16.1770747160769,21.));
#14833=CARTESIAN_POINT('Ctrl Pts',(-9.59446643316596,16.1931534965272,0.));
#14834=CARTESIAN_POINT('Ctrl Pts',(-9.59446643316596,16.1931534965272,21.));
#14835=CARTESIAN_POINT('Ctrl Pts',(-9.60981421781524,16.2168537871666,0.));
#14836=CARTESIAN_POINT('Ctrl Pts',(-9.60981421781524,16.2168537871666,21.));
#14837=CARTESIAN_POINT('Ctrl Pts',(-9.63146315443273,16.2476599387841,0.));
#14838=CARTESIAN_POINT('Ctrl Pts',(-9.63146315443273,16.2476599387841,21.));
#14839=CARTESIAN_POINT('Ctrl Pts',(-9.66014786078746,16.2850845948324,0.));
#14840=CARTESIAN_POINT('Ctrl Pts',(-9.66014786078746,16.2850845948324,21.));
#14841=CARTESIAN_POINT('Ctrl Pts',(-9.69000797146315,16.3217321000366,0.));
#14842=CARTESIAN_POINT('Ctrl Pts',(-9.69000797146315,16.3217321000366,21.));
#14843=CARTESIAN_POINT('Ctrl Pts',(-9.72060002001012,16.3579039682519,0.));
#14844=CARTESIAN_POINT('Ctrl Pts',(-9.72060002001012,16.3579039682519,21.));
#14845=CARTESIAN_POINT('Ctrl Pts',(-9.75159288382684,16.3938231282759,0.));
#14846=CARTESIAN_POINT('Ctrl Pts',(-9.75159288382684,16.3938231282759,21.));
#14847=CARTESIAN_POINT('Ctrl Pts',(-9.78285689698057,16.4295725710378,0.));
#14848=CARTESIAN_POINT('Ctrl Pts',(-9.78285689698057,16.4295725710378,21.));
#14849=CARTESIAN_POINT('Ctrl Pts',(-9.81439757053278,16.4651416449558,0.));
#14850=CARTESIAN_POINT('Ctrl Pts',(-9.81439757053278,16.4651416449558,21.));
#14851=CARTESIAN_POINT('Ctrl Pts',(-9.84630229363521,16.5004633692332,0.));
#14852=CARTESIAN_POINT('Ctrl Pts',(-9.84630229363521,16.5004633692332,21.));
#14853=CARTESIAN_POINT('Ctrl Pts',(-9.8786843754698,16.5354535643506,0.));
#14854=CARTESIAN_POINT('Ctrl Pts',(-9.8786843754698,16.5354535643506,21.));
#14855=CARTESIAN_POINT('Ctrl Pts',(-9.91162317616648,16.5700527532381,0.));
#14856=CARTESIAN_POINT('Ctrl Pts',(-9.91162317616648,16.5700527532381,21.));
#14857=CARTESIAN_POINT('Ctrl Pts',(-9.9451214271291,16.6042559779574,0.));
#14858=CARTESIAN_POINT('Ctrl Pts',(-9.9451214271291,16.6042559779574,21.));
#14859=CARTESIAN_POINT('Ctrl Pts',(-9.97913546489641,16.6380914029057,0.));
#14860=CARTESIAN_POINT('Ctrl Pts',(-9.97913546489641,16.6380914029057,21.));
#14861=CARTESIAN_POINT('Ctrl Pts',(-10.0135950379525,16.6716062376277,0.));
#14862=CARTESIAN_POINT('Ctrl Pts',(-10.0135950379525,16.6716062376277,21.));
#14863=CARTESIAN_POINT('Ctrl Pts',(-10.0484259314257,16.7048506904207,0.));
#14864=CARTESIAN_POINT('Ctrl Pts',(-10.0484259314257,16.7048506904207,21.));
#14865=CARTESIAN_POINT('Ctrl Pts',(-10.0835742491038,16.7378607357337,0.));
#14866=CARTESIAN_POINT('Ctrl Pts',(-10.0835742491038,16.7378607357337,21.));
#14867=CARTESIAN_POINT('Ctrl Pts',(-10.1190207721353,16.7706479198888,0.));
#14868=CARTESIAN_POINT('Ctrl Pts',(-10.1190207721353,16.7706479198888,21.));
#14869=CARTESIAN_POINT('Ctrl Pts',(-10.1547673397274,16.8032089941901,0.));
#14870=CARTESIAN_POINT('Ctrl Pts',(-10.1547673397274,16.8032089941901,21.));
#14871=CARTESIAN_POINT('Ctrl Pts',(-10.1908283166713,16.8355319435838,0.));
#14872=CARTESIAN_POINT('Ctrl Pts',(-10.1908283166713,16.8355319435838,21.));
#14873=CARTESIAN_POINT('Ctrl Pts',(-10.2272206796636,16.8676029947679,0.));
#14874=CARTESIAN_POINT('Ctrl Pts',(-10.2272206796636,16.8676029947679,21.));
#14875=CARTESIAN_POINT('Ctrl Pts',(-10.2639532144219,16.8994142530447,0.));
#14876=CARTESIAN_POINT('Ctrl Pts',(-10.2639532144219,16.8994142530447,21.));
#14877=CARTESIAN_POINT('Ctrl Pts',(-10.3010210756062,16.9309675442426,0.));
#14878=CARTESIAN_POINT('Ctrl Pts',(-10.3010210756062,16.9309675442426,21.));
#14879=CARTESIAN_POINT('Ctrl Pts',(-10.3384116178624,16.9622702798438,0.));
#14880=CARTESIAN_POINT('Ctrl Pts',(-10.3384116178624,16.9622702798438,21.));
#14881=CARTESIAN_POINT('Ctrl Pts',(-10.3761078860454,16.9933329788855,0.));
#14882=CARTESIAN_POINT('Ctrl Pts',(-10.3761078860454,16.9933329788855,21.));
#14883=CARTESIAN_POINT('Ctrl Pts',(-10.4140927470882,17.0241663361802,0.));
#14884=CARTESIAN_POINT('Ctrl Pts',(-10.4140927470882,17.0241663361802,21.));
#14885=CARTESIAN_POINT('Ctrl Pts',(-10.452353435089,17.0547779975888,0.));
#14886=CARTESIAN_POINT('Ctrl Pts',(-10.452353435089,17.0547779975888,21.));
#14887=CARTESIAN_POINT('Ctrl Pts',(-10.4908835057575,17.0851711712016,0.));
#14888=CARTESIAN_POINT('Ctrl Pts',(-10.4908835057575,17.0851711712016,21.));
#14889=CARTESIAN_POINT('Ctrl Pts',(-10.5296803023445,17.1153464189932,0.));
#14890=CARTESIAN_POINT('Ctrl Pts',(-10.5296803023445,17.1153464189932,21.));
#14891=CARTESIAN_POINT('Ctrl Pts',(-10.5687434234512,17.1453027387554,0.));
#14892=CARTESIAN_POINT('Ctrl Pts',(-10.5687434234512,17.1453027387554,21.));
#14893=CARTESIAN_POINT('Ctrl Pts',(-10.6080729180997,17.1750388395657,0.));
#14894=CARTESIAN_POINT('Ctrl Pts',(-10.6080729180997,17.1750388395657,21.));
#14895=CARTESIAN_POINT('Ctrl Pts',(-10.6476672831754,17.2045545572011,0.));
#14896=CARTESIAN_POINT('Ctrl Pts',(-10.6476672831754,17.2045545572011,21.));
#14897=CARTESIAN_POINT('Ctrl Pts',(-10.6875226650217,17.2338514174709,0.));
#14898=CARTESIAN_POINT('Ctrl Pts',(-10.6875226650217,17.2338514174709,21.));
#14899=CARTESIAN_POINT('Ctrl Pts',(-10.7276339231608,17.2629318816279,0.));
#14900=CARTESIAN_POINT('Ctrl Pts',(-10.7276339231608,17.2629318816279,21.));
#14901=CARTESIAN_POINT('Ctrl Pts',(-10.7679952591482,17.2917988998581,0.));
#14902=CARTESIAN_POINT('Ctrl Pts',(-10.7679952591482,17.2917988998581,21.));
#14903=CARTESIAN_POINT('Ctrl Pts',(-10.8086009632423,17.3204553814537,0.));
#14904=CARTESIAN_POINT('Ctrl Pts',(-10.8086009632423,17.3204553814537,21.));
#14905=CARTESIAN_POINT('Ctrl Pts',(-10.8494462423128,17.3489036079991,0.));
#14906=CARTESIAN_POINT('Ctrl Pts',(-10.8494462423128,17.3489036079991,21.));
#14907=CARTESIAN_POINT('Ctrl Pts',(-10.8905275295837,17.377145012528,0.));
#14908=CARTESIAN_POINT('Ctrl Pts',(-10.8905275295837,17.377145012528,21.));
#14909=CARTESIAN_POINT('Ctrl Pts',(-10.9318420203801,17.405180505413,0.));
#14910=CARTESIAN_POINT('Ctrl Pts',(-10.9318420203801,17.405180505413,21.));
#14911=CARTESIAN_POINT('Ctrl Pts',(-10.9733873885115,17.4330106728622,0.));
#14912=CARTESIAN_POINT('Ctrl Pts',(-10.9733873885115,17.4330106728622,21.));
#14913=CARTESIAN_POINT('Ctrl Pts',(-11.0151614525642,17.460636011184,0.));
#14914=CARTESIAN_POINT('Ctrl Pts',(-11.0151614525642,17.460636011184,21.));
#14915=CARTESIAN_POINT('Ctrl Pts',(-11.0571618040371,17.4880571878157,0.));
#14916=CARTESIAN_POINT('Ctrl Pts',(-11.0571618040371,17.4880571878157,21.));
#14917=CARTESIAN_POINT('Ctrl Pts',(-11.0993856581394,17.5152751467292,0.));
#14918=CARTESIAN_POINT('Ctrl Pts',(-11.0993856581394,17.5152751467292,21.));
#14919=CARTESIAN_POINT('Ctrl Pts',(-11.1418300507683,17.5422909714139,0.));
#14920=CARTESIAN_POINT('Ctrl Pts',(-11.1418300507683,17.5422909714139,21.));
#14921=CARTESIAN_POINT('Ctrl Pts',(-11.1844919535058,17.5691058058227,0.));
#14922=CARTESIAN_POINT('Ctrl Pts',(-11.1844919535058,17.5691058058227,21.));
#14923=CARTESIAN_POINT('Ctrl Pts',(-11.2273684103051,17.5957207597803,0.));
#14924=CARTESIAN_POINT('Ctrl Pts',(-11.2273684103051,17.5957207597803,21.));
#14925=CARTESIAN_POINT('Ctrl Pts',(-11.2704566868205,17.6221368072528,0.));
#14926=CARTESIAN_POINT('Ctrl Pts',(-11.2704566868205,17.6221368072528,21.));
#14927=CARTESIAN_POINT('Ctrl Pts',(-11.3137543310722,17.6483547422688,0.));
#14928=CARTESIAN_POINT('Ctrl Pts',(-11.3137543310722,17.6483547422688,21.));
#14929=CARTESIAN_POINT('Ctrl Pts',(-11.3572590796967,17.674375235974,0.));
#14930=CARTESIAN_POINT('Ctrl Pts',(-11.3572590796967,17.674375235974,21.));
#14931=CARTESIAN_POINT('Ctrl Pts',(-11.4009687970126,17.700198872213,0.));
#14932=CARTESIAN_POINT('Ctrl Pts',(-11.4009687970126,17.700198872213,21.));
#14933=CARTESIAN_POINT('Ctrl Pts',(-11.4448814046804,17.725826190457,0.));
#14934=CARTESIAN_POINT('Ctrl Pts',(-11.4448814046804,17.725826190457,21.));
#14935=CARTESIAN_POINT('Ctrl Pts',(-11.4889948016216,17.7512577332768,0.));
#14936=CARTESIAN_POINT('Ctrl Pts',(-11.4889948016216,17.7512577332768,21.));
#14937=CARTESIAN_POINT('Ctrl Pts',(-11.5333068279911,17.7764940721306,0.));
#14938=CARTESIAN_POINT('Ctrl Pts',(-11.5333068279911,17.7764940721306,21.));
#14939=CARTESIAN_POINT('Ctrl Pts',(-11.5778153222435,17.8015357852426,0.));
#14940=CARTESIAN_POINT('Ctrl Pts',(-11.5778153222435,17.8015357852426,21.));
#14941=CARTESIAN_POINT('Ctrl Pts',(-11.6225181583564,17.8263834470057,0.));
#14942=CARTESIAN_POINT('Ctrl Pts',(-11.6225181583564,17.8263834470057,21.));
#14943=CARTESIAN_POINT('Ctrl Pts',(-11.6674132861792,17.8510376144926,0.));
#14944=CARTESIAN_POINT('Ctrl Pts',(-11.6674132861792,17.8510376144926,21.));
#14945=CARTESIAN_POINT('Ctrl Pts',(-11.7124987772363,17.8754988158862,0.));
#14946=CARTESIAN_POINT('Ctrl Pts',(-11.7124987772363,17.8754988158862,21.));
#14947=CARTESIAN_POINT('Ctrl Pts',(-11.7577728408871,17.8997675418752,0.));
#14948=CARTESIAN_POINT('Ctrl Pts',(-11.7577728408871,17.8997675418752,21.));
#14949=CARTESIAN_POINT('Ctrl Pts',(-11.8032337607271,17.9238442458356,0.));
#14950=CARTESIAN_POINT('Ctrl Pts',(-11.8032337607271,17.9238442458356,21.));
#14951=CARTESIAN_POINT('Ctrl Pts',(-11.8488798430201,17.9477293432951,0.));
#14952=CARTESIAN_POINT('Ctrl Pts',(-11.8488798430201,17.9477293432951,21.));
#14953=CARTESIAN_POINT('Ctrl Pts',(-11.8947093631895,17.9714232133203,0.));
#14954=CARTESIAN_POINT('Ctrl Pts',(-11.8947093631895,17.9714232133203,21.));
#14955=CARTESIAN_POINT('Ctrl Pts',(-11.9407205019619,17.9949261997754,0.));
#14956=CARTESIAN_POINT('Ctrl Pts',(-11.9407205019619,17.9949261997754,21.));
#14957=CARTESIAN_POINT('Ctrl Pts',(-11.986911314246,18.0182386160553,0.));
#14958=CARTESIAN_POINT('Ctrl Pts',(-11.986911314246,18.0182386160553,21.));
#14959=CARTESIAN_POINT('Ctrl Pts',(-12.0332798395991,18.0413607600052,0.));
#14960=CARTESIAN_POINT('Ctrl Pts',(-12.0332798395991,18.0413607600052,21.));
#14961=CARTESIAN_POINT('Ctrl Pts',(-12.0798241915081,18.0642929289333,0.));
#14962=CARTESIAN_POINT('Ctrl Pts',(-12.0798241915081,18.0642929289333,21.));
#14963=CARTESIAN_POINT('Ctrl Pts',(-12.1265426519718,18.0870354350128,0.));
#14964=CARTESIAN_POINT('Ctrl Pts',(-12.1265426519718,18.0870354350128,21.));
#14965=CARTESIAN_POINT('Ctrl Pts',(-12.1734337668195,18.109588624154,0.));
#14966=CARTESIAN_POINT('Ctrl Pts',(-12.1734337668195,18.109588624154,21.));
#14967=CARTESIAN_POINT('Ctrl Pts',(-12.2204964278426,18.1319528884305,0.));
#14968=CARTESIAN_POINT('Ctrl Pts',(-12.2204964278426,18.1319528884305,21.));
#14969=CARTESIAN_POINT('Ctrl Pts',(-12.2677298318549,18.1541286139166,0.));
#14970=CARTESIAN_POINT('Ctrl Pts',(-12.2677298318549,18.1541286139166,21.));
#14971=CARTESIAN_POINT('Ctrl Pts',(-12.3056527265146,18.1717186310224,0.));
#14972=CARTESIAN_POINT('Ctrl Pts',(-12.3056527265146,18.1717186310224,21.));
#14973=CARTESIAN_POINT('Ctrl Pts',(-12.3341713636489,18.1848265584754,0.));
#14974=CARTESIAN_POINT('Ctrl Pts',(-12.3341713636489,18.1848265584754,21.));
#14975=CARTESIAN_POINT('Ctrl Pts',(-12.3532177620787,18.1935275957711,0.));
#14976=CARTESIAN_POINT('Ctrl Pts',(-12.3532177620787,18.1935275957711,21.));
#14977=CARTESIAN_POINT('Ctrl Pts',(-12.3627494547115,18.1978687191668,0.));
#14978=CARTESIAN_POINT('Ctrl Pts',(-12.3627494547115,18.1978687191668,21.));
#14979=CARTESIAN_POINT('Ctrl Pts',(-9.57984538049455,16.1689656784104,0.));
#14980=CARTESIAN_POINT('Ctrl Pts',(-9.58464985151482,16.1770747160769,0.));
#14981=CARTESIAN_POINT('Ctrl Pts',(-9.59446643316596,16.1931534965272,0.));
#14982=CARTESIAN_POINT('Ctrl Pts',(-9.60981421781524,16.2168537871666,0.));
#14983=CARTESIAN_POINT('Ctrl Pts',(-9.63146315443273,16.2476599387841,0.));
#14984=CARTESIAN_POINT('Ctrl Pts',(-9.66014786078746,16.2850845948324,0.));
#14985=CARTESIAN_POINT('Ctrl Pts',(-9.69000797146315,16.3217321000366,0.));
#14986=CARTESIAN_POINT('Ctrl Pts',(-9.72060002001012,16.3579039682519,0.));
#14987=CARTESIAN_POINT('Ctrl Pts',(-9.75159288382684,16.3938231282759,0.));
#14988=CARTESIAN_POINT('Ctrl Pts',(-9.78285689698057,16.4295725710378,0.));
#14989=CARTESIAN_POINT('Ctrl Pts',(-9.81439757053278,16.4651416449558,0.));
#14990=CARTESIAN_POINT('Ctrl Pts',(-9.84630229363521,16.5004633692332,0.));
#14991=CARTESIAN_POINT('Ctrl Pts',(-9.8786843754698,16.5354535643506,0.));
#14992=CARTESIAN_POINT('Ctrl Pts',(-9.91162317616648,16.5700527532381,0.));
#14993=CARTESIAN_POINT('Ctrl Pts',(-9.9451214271291,16.6042559779574,0.));
#14994=CARTESIAN_POINT('Ctrl Pts',(-9.97913546489641,16.6380914029057,0.));
#14995=CARTESIAN_POINT('Ctrl Pts',(-10.0135950379525,16.6716062376277,0.));
#14996=CARTESIAN_POINT('Ctrl Pts',(-10.0484259314257,16.7048506904207,0.));
#14997=CARTESIAN_POINT('Ctrl Pts',(-10.0835742491038,16.7378607357337,0.));
#14998=CARTESIAN_POINT('Ctrl Pts',(-10.1190207721353,16.7706479198888,0.));
#14999=CARTESIAN_POINT('Ctrl Pts',(-10.1547673397274,16.8032089941901,0.));
#15000=CARTESIAN_POINT('Ctrl Pts',(-10.1908283166713,16.8355319435838,0.));
#15001=CARTESIAN_POINT('Ctrl Pts',(-10.2272206796636,16.8676029947679,0.));
#15002=CARTESIAN_POINT('Ctrl Pts',(-10.2639532144219,16.8994142530447,0.));
#15003=CARTESIAN_POINT('Ctrl Pts',(-10.3010210756062,16.9309675442426,0.));
#15004=CARTESIAN_POINT('Ctrl Pts',(-10.3384116178624,16.9622702798438,0.));
#15005=CARTESIAN_POINT('Ctrl Pts',(-10.3761078860454,16.9933329788855,0.));
#15006=CARTESIAN_POINT('Ctrl Pts',(-10.4140927470882,17.0241663361802,0.));
#15007=CARTESIAN_POINT('Ctrl Pts',(-10.452353435089,17.0547779975888,0.));
#15008=CARTESIAN_POINT('Ctrl Pts',(-10.4908835057575,17.0851711712016,0.));
#15009=CARTESIAN_POINT('Ctrl Pts',(-10.5296803023445,17.1153464189932,0.));
#15010=CARTESIAN_POINT('Ctrl Pts',(-10.5687434234512,17.1453027387554,0.));
#15011=CARTESIAN_POINT('Ctrl Pts',(-10.6080729180997,17.1750388395657,0.));
#15012=CARTESIAN_POINT('Ctrl Pts',(-10.6476672831754,17.2045545572011,0.));
#15013=CARTESIAN_POINT('Ctrl Pts',(-10.6875226650217,17.2338514174709,0.));
#15014=CARTESIAN_POINT('Ctrl Pts',(-10.7276339231608,17.2629318816279,0.));
#15015=CARTESIAN_POINT('Ctrl Pts',(-10.7679952591482,17.2917988998581,0.));
#15016=CARTESIAN_POINT('Ctrl Pts',(-10.8086009632423,17.3204553814537,0.));
#15017=CARTESIAN_POINT('Ctrl Pts',(-10.8494462423128,17.3489036079991,0.));
#15018=CARTESIAN_POINT('Ctrl Pts',(-10.8905275295837,17.377145012528,0.));
#15019=CARTESIAN_POINT('Ctrl Pts',(-10.9318420203801,17.405180505413,0.));
#15020=CARTESIAN_POINT('Ctrl Pts',(-10.9733873885115,17.4330106728622,0.));
#15021=CARTESIAN_POINT('Ctrl Pts',(-11.0151614525642,17.460636011184,0.));
#15022=CARTESIAN_POINT('Ctrl Pts',(-11.0571618040371,17.4880571878157,0.));
#15023=CARTESIAN_POINT('Ctrl Pts',(-11.0993856581394,17.5152751467292,0.));
#15024=CARTESIAN_POINT('Ctrl Pts',(-11.1418300507683,17.5422909714139,0.));
#15025=CARTESIAN_POINT('Ctrl Pts',(-11.1844919535058,17.5691058058227,0.));
#15026=CARTESIAN_POINT('Ctrl Pts',(-11.2273684103051,17.5957207597803,0.));
#15027=CARTESIAN_POINT('Ctrl Pts',(-11.2704566868205,17.6221368072528,0.));
#15028=CARTESIAN_POINT('Ctrl Pts',(-11.3137543310722,17.6483547422688,0.));
#15029=CARTESIAN_POINT('Ctrl Pts',(-11.3572590796967,17.674375235974,0.));
#15030=CARTESIAN_POINT('Ctrl Pts',(-11.4009687970126,17.700198872213,0.));
#15031=CARTESIAN_POINT('Ctrl Pts',(-11.4448814046804,17.725826190457,0.));
#15032=CARTESIAN_POINT('Ctrl Pts',(-11.4889948016216,17.7512577332768,0.));
#15033=CARTESIAN_POINT('Ctrl Pts',(-11.5333068279911,17.7764940721306,0.));
#15034=CARTESIAN_POINT('Ctrl Pts',(-11.5778153222435,17.8015357852426,0.));
#15035=CARTESIAN_POINT('Ctrl Pts',(-11.6225181583564,17.8263834470057,0.));
#15036=CARTESIAN_POINT('Ctrl Pts',(-11.6674132861792,17.8510376144926,0.));
#15037=CARTESIAN_POINT('Ctrl Pts',(-11.7124987772363,17.8754988158862,0.));
#15038=CARTESIAN_POINT('Ctrl Pts',(-11.7577728408871,17.8997675418752,0.));
#15039=CARTESIAN_POINT('Ctrl Pts',(-11.8032337607271,17.9238442458356,0.));
#15040=CARTESIAN_POINT('Ctrl Pts',(-11.8488798430201,17.9477293432951,0.));
#15041=CARTESIAN_POINT('Ctrl Pts',(-11.8947093631895,17.9714232133203,0.));
#15042=CARTESIAN_POINT('Ctrl Pts',(-11.9407205019619,17.9949261997754,0.));
#15043=CARTESIAN_POINT('Ctrl Pts',(-11.986911314246,18.0182386160553,0.));
#15044=CARTESIAN_POINT('Ctrl Pts',(-12.0332798395991,18.0413607600052,0.));
#15045=CARTESIAN_POINT('Ctrl Pts',(-12.0798241915081,18.0642929289333,0.));
#15046=CARTESIAN_POINT('Ctrl Pts',(-12.1265426519718,18.0870354350128,0.));
#15047=CARTESIAN_POINT('Ctrl Pts',(-12.1734337668195,18.109588624154,0.));
#15048=CARTESIAN_POINT('Ctrl Pts',(-12.2299089600472,18.1364257412858,0.));
#15049=CARTESIAN_POINT('Ctrl Pts',(-12.2771850498068,18.1585543320743,0.));
#15050=CARTESIAN_POINT('Ctrl Pts',(-12.3151419520839,18.1761067306718,0.));
#15051=CARTESIAN_POINT('Ctrl Pts',(-12.3436860694314,18.1891864723772,0.));
#15052=CARTESIAN_POINT('Ctrl Pts',(-12.3627494547115,18.1978687191668,0.));
#15053=CARTESIAN_POINT('Ctrl Pts',(-9.57984538049455,16.1689656784104,13.));
#15054=CARTESIAN_POINT('Ctrl Pts',(-9.58794311444298,16.1826331205334,13.));
#15055=CARTESIAN_POINT('Ctrl Pts',(-9.59639855902712,16.1960605405031,13.));
#15056=CARTESIAN_POINT('Ctrl Pts',(-9.60518801711085,16.209264165571,13.));
#15057=CARTESIAN_POINT('Ctrl Pts',(-9.6154899193841,16.224739801703,13.));
#15058=CARTESIAN_POINT('Ctrl Pts',(-9.62624998107167,16.2399084848584,13.));
#15059=CARTESIAN_POINT('Ctrl Pts',(-9.63737105568732,16.254836637175,13.));
#15060=CARTESIAN_POINT('Ctrl Pts',(-9.65301893989002,16.2758412618972,13.));
#15061=CARTESIAN_POINT('Ctrl Pts',(-9.66937567449949,16.296373798599,13.));
#15062=CARTESIAN_POINT('Ctrl Pts',(-9.68610238201322,16.3166650331518,13.));
#15063=CARTESIAN_POINT('Ctrl Pts',(-9.69722828051063,16.3301619042985,13.));
#15064=CARTESIAN_POINT('Ctrl Pts',(-9.70851618070807,16.3435531467518,13.));
#15065=CARTESIAN_POINT('Ctrl Pts',(-9.7198910779208,16.3568892752788,13.));
#15066=CARTESIAN_POINT('Ctrl Pts',(-9.73186502184932,16.3709277366574,13.));
#15067=CARTESIAN_POINT('Ctrl Pts',(-9.74393463776872,16.3849056240572,13.));
#15068=CARTESIAN_POINT('Ctrl Pts',(-9.75606525513648,16.3988451548219,13.));
#15069=CARTESIAN_POINT('Ctrl Pts',(-9.76953696975778,16.414325766791,13.));
#15070=CARTESIAN_POINT('Ctrl Pts',(-9.78308498747417,16.4297583183324,13.));
#15071=CARTESIAN_POINT('Ctrl Pts',(-9.79671869019648,16.4451338763398,13.));
#15072=CARTESIAN_POINT('Ctrl Pts',(-9.8172721587789,16.4683132763075,13.));
#15073=CARTESIAN_POINT('Ctrl Pts',(-9.83802550134249,16.4913594464712,13.));
#15074=CARTESIAN_POINT('Ctrl Pts',(-9.85910360864921,16.5141788054336,13.));
#15075=CARTESIAN_POINT('Ctrl Pts',(-9.87441639279172,16.5307565708362,13.));
#15076=CARTESIAN_POINT('Ctrl Pts',(-9.88990330206224,16.5472127770975,13.));
#15077=CARTESIAN_POINT('Ctrl Pts',(-9.90558047214324,16.5635345032205,13.));
#15078=CARTESIAN_POINT('Ctrl Pts',(-9.92474447016175,16.5834864158081,13.));
#15079=CARTESIAN_POINT('Ctrl Pts',(-9.9441917311001,16.6032381063718,13.));
#15080=CARTESIAN_POINT('Ctrl Pts',(-9.96388214930656,16.6228156007807,13.));
#15081=CARTESIAN_POINT('Ctrl Pts',(-9.9851510689085,16.6439625439398,13.));
#15082=CARTESIAN_POINT('Ctrl Pts',(-10.006698815053,16.6649096998191,13.));
#15083=CARTESIAN_POINT('Ctrl Pts',(-10.0284493480904,16.6857083247995,13.));
#15084=CARTESIAN_POINT('Ctrl Pts',(-10.0485293380076,16.7049095176705,13.));
#15085=CARTESIAN_POINT('Ctrl Pts',(-10.0687801145851,16.7239855768682,13.));
#15086=CARTESIAN_POINT('Ctrl Pts',(-10.0891775910162,16.7429517500628,13.));
#15087=CARTESIAN_POINT('Ctrl Pts',(-10.1168886100216,16.7687182701337,13.));
#15088=CARTESIAN_POINT('Ctrl Pts',(-10.1448719871919,16.7942808297111,13.));
#15089=CARTESIAN_POINT('Ctrl Pts',(-10.1731502199822,16.8196194580034,13.));
#15090=CARTESIAN_POINT('Ctrl Pts',(-10.2004381038963,16.844070687064,13.));
#15091=CARTESIAN_POINT('Ctrl Pts',(-10.2280069309447,16.8683088890975,13.));
#15092=CARTESIAN_POINT('Ctrl Pts',(-10.2558682820918,16.8923226175541,13.));
#15093=CARTESIAN_POINT('Ctrl Pts',(-10.2937187080479,16.9249459403096,13.));
#15094=CARTESIAN_POINT('Ctrl Pts',(-10.3321063567812,16.9571568356211,13.));
#15095=CARTESIAN_POINT('Ctrl Pts',(-10.3709578724058,16.9889999235317,13.));
#15096=CARTESIAN_POINT('Ctrl Pts',(-10.4051075100498,17.0169893055707,13.));
#15097=CARTESIAN_POINT('Ctrl Pts',(-10.4396099589146,17.04469848632,13.));
#15098=CARTESIAN_POINT('Ctrl Pts',(-10.474436876203,17.0721430001642,13.));
#15099=CARTESIAN_POINT('Ctrl Pts',(-10.5257802081583,17.112602877017,13.));
#15100=CARTESIAN_POINT('Ctrl Pts',(-10.5778361036082,17.1524822680152,13.));
#15101=CARTESIAN_POINT('Ctrl Pts',(-10.6305946314222,17.1917748564523,13.));
#15102=CARTESIAN_POINT('Ctrl Pts',(-10.6971764080832,17.2413624862848,13.));
#15103=CARTESIAN_POINT('Ctrl Pts',(-10.7648729797973,17.2900185098528,13.));
#15104=CARTESIAN_POINT('Ctrl Pts',(-10.8335716334697,17.3377983051247,13.));
#15105=CARTESIAN_POINT('Ctrl Pts',(-10.9266292559136,17.4025197212104,13.));
#15106=CARTESIAN_POINT('Ctrl Pts',(-11.0215303643735,17.465629946501,13.));
#15107=CARTESIAN_POINT('Ctrl Pts',(-11.1181400554829,17.5271690583862,13.));
#15108=CARTESIAN_POINT('Ctrl Pts',(-11.2042701255893,17.5820327885162,13.));
#15109=CARTESIAN_POINT('Ctrl Pts',(-11.2917512652755,17.6356526662346,13.));
#15110=CARTESIAN_POINT('Ctrl Pts',(-11.3804891386083,17.6880597469658,13.));
#15111=CARTESIAN_POINT('Ctrl Pts',(-11.5062551071101,17.7623349917623,13.));
#15112=CARTESIAN_POINT('Ctrl Pts',(-11.6345494475067,17.8341701535583,13.));
#15113=CARTESIAN_POINT('Ctrl Pts',(-11.7651542350891,17.9036238122623,13.));
#15114=CARTESIAN_POINT('Ctrl Pts',(-11.8666049261148,17.9575737615728,13.));
#15115=CARTESIAN_POINT('Ctrl Pts',(-11.9694546915569,18.0100864746768,13.));
#15116=CARTESIAN_POINT('Ctrl Pts',(-12.0736101881878,18.0611784501095,13.));
#15117=CARTESIAN_POINT('Ctrl Pts',(-12.163712553743,18.1053768649439,13.));
#15118=CARTESIAN_POINT('Ctrl Pts',(-12.2547877895871,18.1485120955669,13.));
#15119=CARTESIAN_POINT('Ctrl Pts',(-12.346811245556,18.1905949538241,13.));
#15120=CARTESIAN_POINT('Ctrl Pts',(-12.3521208117116,18.1930230491134,13.));
#15121=CARTESIAN_POINT('Ctrl Pts',(-12.357433548157,18.1954476374973,13.));
#15122=CARTESIAN_POINT('Ctrl Pts',(-12.3627494547115,18.1978687191668,13.));
#15123=CARTESIAN_POINT('Ctrl Pts',(-7.45574324794401,20.698113262342,0.));
#15124=CARTESIAN_POINT('Ctrl Pts',(-7.45574324794401,20.698113262342,21.));
#15125=CARTESIAN_POINT('Ctrl Pts',(-7.45783379370107,20.6878503127065,0.));
#15126=CARTESIAN_POINT('Ctrl Pts',(-7.45783379370107,20.6878503127065,21.));
#15127=CARTESIAN_POINT('Ctrl Pts',(-7.46198969876653,20.6673271112931,0.));
#15128=CARTESIAN_POINT('Ctrl Pts',(-7.46198969876653,20.6673271112931,21.));
#15129=CARTESIAN_POINT('Ctrl Pts',(-7.46814799701905,20.6365504027501,0.));
#15130=CARTESIAN_POINT('Ctrl Pts',(-7.46814799701905,20.6365504027501,21.));
#15131=CARTESIAN_POINT('Ctrl Pts',(-7.47620789245427,20.5955309838521,0.));
#15132=CARTESIAN_POINT('Ctrl Pts',(-7.47620789245427,20.5955309838521,21.));
#15133=CARTESIAN_POINT('Ctrl Pts',(-7.48603045196744,20.5442837929044,0.));
#15134=CARTESIAN_POINT('Ctrl Pts',(-7.48603045196744,20.5442837929044,21.));
#15135=CARTESIAN_POINT('Ctrl Pts',(-7.49560012018405,20.4930639156161,0.));
#15136=CARTESIAN_POINT('Ctrl Pts',(-7.49560012018405,20.4930639156161,21.));
#15137=CARTESIAN_POINT('Ctrl Pts',(-7.50491611266253,20.4418717748497,0.));
#15138=CARTESIAN_POINT('Ctrl Pts',(-7.50491611266253,20.4418717748497,21.));
#15139=CARTESIAN_POINT('Ctrl Pts',(-7.51397746081993,20.3907080367098,0.));
#15140=CARTESIAN_POINT('Ctrl Pts',(-7.51397746081993,20.3907080367098,21.));
#15141=CARTESIAN_POINT('Ctrl Pts',(-7.52278303006887,20.3395736743243,0.));
#15142=CARTESIAN_POINT('Ctrl Pts',(-7.52278303006887,20.3395736743243,21.));
#15143=CARTESIAN_POINT('Ctrl Pts',(-7.53133155804007,20.2884698940944,0.));
#15144=CARTESIAN_POINT('Ctrl Pts',(-7.53133155804007,20.2884698940944,21.));
#15145=CARTESIAN_POINT('Ctrl Pts',(-7.53962169534166,20.2373980474879,0.));
#15146=CARTESIAN_POINT('Ctrl Pts',(-7.53962169534166,20.2373980474879,21.));
#15147=CARTESIAN_POINT('Ctrl Pts',(-7.54765204869254,20.1863595454674,0.));
#15148=CARTESIAN_POINT('Ctrl Pts',(-7.54765204869254,20.1863595454674,21.));
#15149=CARTESIAN_POINT('Ctrl Pts',(-7.55542122125494,20.1353557774357,0.));
#15150=CARTESIAN_POINT('Ctrl Pts',(-7.55542122125494,20.1353557774357,21.));
#15151=CARTESIAN_POINT('Ctrl Pts',(-7.5629278654946,20.0843880130978,0.));
#15152=CARTESIAN_POINT('Ctrl Pts',(-7.5629278654946,20.0843880130978,21.));
#15153=CARTESIAN_POINT('Ctrl Pts',(-7.57017066105973,20.0334574248556,0.));
#15154=CARTESIAN_POINT('Ctrl Pts',(-7.57017066105973,20.0334574248556,21.));
#15155=CARTESIAN_POINT('Ctrl Pts',(-7.57714827622806,19.9825651387294,0.));
#15156=CARTESIAN_POINT('Ctrl Pts',(-7.57714827622806,19.9825651387294,21.));
#15157=CARTESIAN_POINT('Ctrl Pts',(-7.58385933533351,19.931712276832,0.));
#15158=CARTESIAN_POINT('Ctrl Pts',(-7.58385933533351,19.931712276832,21.));
#15159=CARTESIAN_POINT('Ctrl Pts',(-7.59030238888852,19.8808999994024,0.));
#15160=CARTESIAN_POINT('Ctrl Pts',(-7.59030238888852,19.8808999994024,21.));
#15161=CARTESIAN_POINT('Ctrl Pts',(-7.59647587605448,19.830129556152,0.));
#15162=CARTESIAN_POINT('Ctrl Pts',(-7.59647587605448,19.830129556152,21.));
#15163=CARTESIAN_POINT('Ctrl Pts',(-7.60237814110186,19.7794022782484,0.));
#15164=CARTESIAN_POINT('Ctrl Pts',(-7.60237814110186,19.7794022782484,21.));
#15165=CARTESIAN_POINT('Ctrl Pts',(-7.60800746969261,19.7287195480601,0.));
#15166=CARTESIAN_POINT('Ctrl Pts',(-7.60800746969261,19.7287195480601,21.));
#15167=CARTESIAN_POINT('Ctrl Pts',(-7.61336212350879,19.6780827744426,0.));
#15168=CARTESIAN_POINT('Ctrl Pts',(-7.61336212350879,19.6780827744426,21.));
#15169=CARTESIAN_POINT('Ctrl Pts',(-7.6184403707059,19.6274933688524,0.));
#15170=CARTESIAN_POINT('Ctrl Pts',(-7.6184403707059,19.6274933688524,21.));
#15171=CARTESIAN_POINT('Ctrl Pts',(-7.62324053735219,19.5769527121826,0.));
#15172=CARTESIAN_POINT('Ctrl Pts',(-7.62324053735219,19.5769527121826,21.));
#15173=CARTESIAN_POINT('Ctrl Pts',(-7.62776096538882,19.5264621687521,0.));
#15174=CARTESIAN_POINT('Ctrl Pts',(-7.62776096538882,19.5264621687521,21.));
#15175=CARTESIAN_POINT('Ctrl Pts',(-7.63199992715365,19.4760231231881,0.));
#15176=CARTESIAN_POINT('Ctrl Pts',(-7.63199992715365,19.4760231231881,21.));
#15177=CARTESIAN_POINT('Ctrl Pts',(-7.63595554930654,19.4256370121006,0.));
#15178=CARTESIAN_POINT('Ctrl Pts',(-7.63595554930654,19.4256370121006,21.));
#15179=CARTESIAN_POINT('Ctrl Pts',(-7.6396257482276,19.3753053524647,0.));
#15180=CARTESIAN_POINT('Ctrl Pts',(-7.6396257482276,19.3753053524647,21.));
#15181=CARTESIAN_POINT('Ctrl Pts',(-7.64300812875338,19.3250297839295,0.));
#15182=CARTESIAN_POINT('Ctrl Pts',(-7.64300812875338,19.3250297839295,21.));
#15183=CARTESIAN_POINT('Ctrl Pts',(-7.64610005549613,19.2748120456486,0.));
#15184=CARTESIAN_POINT('Ctrl Pts',(-7.64610005549613,19.2748120456486,21.));
#15185=CARTESIAN_POINT('Ctrl Pts',(-7.64889882291923,19.224653915265,0.));
#15186=CARTESIAN_POINT('Ctrl Pts',(-7.64889882291923,19.224653915265,21.));
#15187=CARTESIAN_POINT('Ctrl Pts',(-7.65140181220525,19.1745571539291,0.));
#15188=CARTESIAN_POINT('Ctrl Pts',(-7.65140181220525,19.1745571539291,21.));
#15189=CARTESIAN_POINT('Ctrl Pts',(-7.65360662280609,19.1245234597312,0.));
#15190=CARTESIAN_POINT('Ctrl Pts',(-7.65360662280609,19.1245234597312,21.));
#15191=CARTESIAN_POINT('Ctrl Pts',(-7.65551129907201,19.0745543888799,0.));
#15192=CARTESIAN_POINT('Ctrl Pts',(-7.65551129907201,19.0745543888799,21.));
#15193=CARTESIAN_POINT('Ctrl Pts',(-7.65711415727855,19.0246514144531,0.));
#15194=CARTESIAN_POINT('Ctrl Pts',(-7.65711415727855,19.0246514144531,21.));
#15195=CARTESIAN_POINT('Ctrl Pts',(-7.65841335587266,18.974816073814,0.));
#15196=CARTESIAN_POINT('Ctrl Pts',(-7.65841335587266,18.974816073814,21.));
#15197=CARTESIAN_POINT('Ctrl Pts',(-7.65940650980098,18.9250501008887,0.));
#15198=CARTESIAN_POINT('Ctrl Pts',(-7.65940650980098,18.9250501008887,21.));
#15199=CARTESIAN_POINT('Ctrl Pts',(-7.66009036321663,18.8753555389435,0.));
#15200=CARTESIAN_POINT('Ctrl Pts',(-7.66009036321663,18.8753555389435,21.));
#15201=CARTESIAN_POINT('Ctrl Pts',(-7.66046025294774,18.8257349246207,0.));
#15202=CARTESIAN_POINT('Ctrl Pts',(-7.66046025294774,18.8257349246207,21.));
#15203=CARTESIAN_POINT('Ctrl Pts',(-7.6605104692254,18.7761911671591,0.));
#15204=CARTESIAN_POINT('Ctrl Pts',(-7.6605104692254,18.7761911671591,21.));
#15205=CARTESIAN_POINT('Ctrl Pts',(-7.66023521705904,18.7267272235231,0.));
#15206=CARTESIAN_POINT('Ctrl Pts',(-7.66023521705904,18.7267272235231,21.));
#15207=CARTESIAN_POINT('Ctrl Pts',(-7.65962948375621,18.6773458057584,0.));
#15208=CARTESIAN_POINT('Ctrl Pts',(-7.65962948375621,18.6773458057584,21.));
#15209=CARTESIAN_POINT('Ctrl Pts',(-7.65868976978872,18.6280491346907,0.));
#15210=CARTESIAN_POINT('Ctrl Pts',(-7.65868976978872,18.6280491346907,21.));
#15211=CARTESIAN_POINT('Ctrl Pts',(-7.65741532450727,18.5788385228928,0.));
#15212=CARTESIAN_POINT('Ctrl Pts',(-7.65741532450727,18.5788385228928,21.));
#15213=CARTESIAN_POINT('Ctrl Pts',(-7.65580722110436,18.5297146894905,0.));
#15214=CARTESIAN_POINT('Ctrl Pts',(-7.65580722110436,18.5297146894905,21.));
#15215=CARTESIAN_POINT('Ctrl Pts',(-7.65386603444742,18.4806785483052,0.));
#15216=CARTESIAN_POINT('Ctrl Pts',(-7.65386603444742,18.4806785483052,21.));
#15217=CARTESIAN_POINT('Ctrl Pts',(-7.65158974829126,18.4317319183719,0.));
#15218=CARTESIAN_POINT('Ctrl Pts',(-7.65158974829126,18.4317319183719,21.));
#15219=CARTESIAN_POINT('Ctrl Pts',(-7.6489719793775,18.3828781275628,0.));
#15220=CARTESIAN_POINT('Ctrl Pts',(-7.6489719793775,18.3828781275628,21.));
#15221=CARTESIAN_POINT('Ctrl Pts',(-7.64599903846601,18.3341230095852,0.));
#15222=CARTESIAN_POINT('Ctrl Pts',(-7.64599903846601,18.3341230095852,21.));
#15223=CARTESIAN_POINT('Ctrl Pts',(-7.6426522027076,18.2854741391282,0.));
#15224=CARTESIAN_POINT('Ctrl Pts',(-7.6426522027076,18.2854741391282,21.));
#15225=CARTESIAN_POINT('Ctrl Pts',(-7.63891299603826,18.2369390502576,0.));
#15226=CARTESIAN_POINT('Ctrl Pts',(-7.63891299603826,18.2369390502576,21.));
#15227=CARTESIAN_POINT('Ctrl Pts',(-7.63476798969016,18.1885236169197,0.));
#15228=CARTESIAN_POINT('Ctrl Pts',(-7.63476798969016,18.1885236169197,21.));
#15229=CARTESIAN_POINT('Ctrl Pts',(-7.63021285851761,18.1402306858819,0.));
#15230=CARTESIAN_POINT('Ctrl Pts',(-7.63021285851761,18.1402306858819,21.));
#15231=CARTESIAN_POINT('Ctrl Pts',(-7.62525915358073,18.0920577897363,0.));
#15232=CARTESIAN_POINT('Ctrl Pts',(-7.62525915358073,18.0920577897363,21.));
#15233=CARTESIAN_POINT('Ctrl Pts',(-7.61992799636654,18.0439992897906,0.));
#15234=CARTESIAN_POINT('Ctrl Pts',(-7.61992799636654,18.0439992897906,21.));
#15235=CARTESIAN_POINT('Ctrl Pts',(-7.61423755067037,17.9960506269561,0.));
#15236=CARTESIAN_POINT('Ctrl Pts',(-7.61423755067037,17.9960506269561,21.));
#15237=CARTESIAN_POINT('Ctrl Pts',(-7.60819152580111,17.9482122228183,0.));
#15238=CARTESIAN_POINT('Ctrl Pts',(-7.60819152580111,17.9482122228183,21.));
#15239=CARTESIAN_POINT('Ctrl Pts',(-7.60176928403058,17.900492838997,0.));
#15240=CARTESIAN_POINT('Ctrl Pts',(-7.60176928403058,17.900492838997,21.));
#15241=CARTESIAN_POINT('Ctrl Pts',(-7.59491004201955,17.8529149331931,0.));
#15242=CARTESIAN_POINT('Ctrl Pts',(-7.59491004201955,17.8529149331931,21.));
#15243=CARTESIAN_POINT('Ctrl Pts',(-7.58752955799499,17.8055090348024,0.));
#15244=CARTESIAN_POINT('Ctrl Pts',(-7.58752955799499,17.8055090348024,21.));
#15245=CARTESIAN_POINT('Ctrl Pts',(-7.57954834582803,17.7583042294209,0.));
#15246=CARTESIAN_POINT('Ctrl Pts',(-7.57954834582803,17.7583042294209,21.));
#15247=CARTESIAN_POINT('Ctrl Pts',(-7.57091795530423,17.7113192869136,0.));
#15248=CARTESIAN_POINT('Ctrl Pts',(-7.57091795530423,17.7113192869136,21.));
#15249=CARTESIAN_POINT('Ctrl Pts',(-7.56164400295862,17.6645549117314,0.));
#15250=CARTESIAN_POINT('Ctrl Pts',(-7.56164400295862,17.6645549117314,21.));
#15251=CARTESIAN_POINT('Ctrl Pts',(-7.55182125346563,17.6179818599248,0.));
#15252=CARTESIAN_POINT('Ctrl Pts',(-7.55182125346563,17.6179818599248,21.));
#15253=CARTESIAN_POINT('Ctrl Pts',(-7.54158441095317,17.5715579419204,0.));
#15254=CARTESIAN_POINT('Ctrl Pts',(-7.54158441095317,17.5715579419204,21.));
#15255=CARTESIAN_POINT('Ctrl Pts',(-7.53103903007863,17.5252518287336,0.));
#15256=CARTESIAN_POINT('Ctrl Pts',(-7.53103903007863,17.5252518287336,21.));
#15257=CARTESIAN_POINT('Ctrl Pts',(-7.52019696747328,17.4790653226646,0.));
#15258=CARTESIAN_POINT('Ctrl Pts',(-7.52019696747328,17.4790653226646,21.));
#15259=CARTESIAN_POINT('Ctrl Pts',(-7.50891486634214,17.4330545448126,0.));
#15260=CARTESIAN_POINT('Ctrl Pts',(-7.50891486634214,17.4330545448126,21.));
#15261=CARTESIAN_POINT('Ctrl Pts',(-7.4968177445175,17.3873563447297,0.));
#15262=CARTESIAN_POINT('Ctrl Pts',(-7.4968177445175,17.3873563447297,21.));
#15263=CARTESIAN_POINT('Ctrl Pts',(-7.48340100912745,17.3421522689127,0.));
#15264=CARTESIAN_POINT('Ctrl Pts',(-7.48340100912745,17.3421522689127,21.));
#15265=CARTESIAN_POINT('Ctrl Pts',(-7.47120323460919,17.3065305096784,0.));
#15266=CARTESIAN_POINT('Ctrl Pts',(-7.47120323460919,17.3065305096784,21.));
#15267=CARTESIAN_POINT('Ctrl Pts',(-7.4610504981825,17.2801832097582,0.));
#15268=CARTESIAN_POINT('Ctrl Pts',(-7.4610504981825,17.2801832097582,21.));
#15269=CARTESIAN_POINT('Ctrl Pts',(-7.45381253347183,17.2627905583523,0.));
#15270=CARTESIAN_POINT('Ctrl Pts',(-7.45381253347183,17.2627905583523,21.));
#15271=CARTESIAN_POINT('Ctrl Pts',(-7.45007618140238,17.2541372868972,0.));
#15272=CARTESIAN_POINT('Ctrl Pts',(-7.45007618140238,17.2541372868972,21.));
#15273=CARTESIAN_POINT('',(-7.45574324794407,20.698113262342,0.));
#15274=CARTESIAN_POINT('Ctrl Pts',(-7.45007618140238,17.2541372868972,0.));
#15275=CARTESIAN_POINT('Ctrl Pts',(-7.45381253347183,17.2627905583523,0.));
#15276=CARTESIAN_POINT('Ctrl Pts',(-7.4610504981825,17.2801832097582,0.));
#15277=CARTESIAN_POINT('Ctrl Pts',(-7.47120323460919,17.3065305096784,0.));
#15278=CARTESIAN_POINT('Ctrl Pts',(-7.48340100912745,17.3421522689127,0.));
#15279=CARTESIAN_POINT('Ctrl Pts',(-7.4968177445175,17.3873563447297,0.));
#15280=CARTESIAN_POINT('Ctrl Pts',(-7.50891486634214,17.4330545448126,0.));
#15281=CARTESIAN_POINT('Ctrl Pts',(-7.52019696747328,17.4790653226646,0.));
#15282=CARTESIAN_POINT('Ctrl Pts',(-7.53103903007863,17.5252518287336,0.));
#15283=CARTESIAN_POINT('Ctrl Pts',(-7.54158441095317,17.5715579419204,0.));
#15284=CARTESIAN_POINT('Ctrl Pts',(-7.55182125346563,17.6179818599248,0.));
#15285=CARTESIAN_POINT('Ctrl Pts',(-7.56164400295862,17.6645549117314,0.));
#15286=CARTESIAN_POINT('Ctrl Pts',(-7.57091795530423,17.7113192869136,0.));
#15287=CARTESIAN_POINT('Ctrl Pts',(-7.57954834582803,17.7583042294209,0.));
#15288=CARTESIAN_POINT('Ctrl Pts',(-7.58752955799499,17.8055090348024,0.));
#15289=CARTESIAN_POINT('Ctrl Pts',(-7.59491004201955,17.8529149331931,0.));
#15290=CARTESIAN_POINT('Ctrl Pts',(-7.60176928403058,17.900492838997,0.));
#15291=CARTESIAN_POINT('Ctrl Pts',(-7.60819152580111,17.9482122228183,0.));
#15292=CARTESIAN_POINT('Ctrl Pts',(-7.61423755067037,17.9960506269561,0.));
#15293=CARTESIAN_POINT('Ctrl Pts',(-7.61992799636654,18.0439992897906,0.));
#15294=CARTESIAN_POINT('Ctrl Pts',(-7.62525915358073,18.0920577897363,0.));
#15295=CARTESIAN_POINT('Ctrl Pts',(-7.63021285851761,18.1402306858819,0.));
#15296=CARTESIAN_POINT('Ctrl Pts',(-7.63476798969016,18.1885236169197,0.));
#15297=CARTESIAN_POINT('Ctrl Pts',(-7.63891299603826,18.2369390502576,0.));
#15298=CARTESIAN_POINT('Ctrl Pts',(-7.6426522027076,18.2854741391282,0.));
#15299=CARTESIAN_POINT('Ctrl Pts',(-7.64599903846601,18.3341230095852,0.));
#15300=CARTESIAN_POINT('Ctrl Pts',(-7.6489719793775,18.3828781275628,0.));
#15301=CARTESIAN_POINT('Ctrl Pts',(-7.65158974829126,18.4317319183719,0.));
#15302=CARTESIAN_POINT('Ctrl Pts',(-7.65386603444742,18.4806785483052,0.));
#15303=CARTESIAN_POINT('Ctrl Pts',(-7.65580722110436,18.5297146894905,0.));
#15304=CARTESIAN_POINT('Ctrl Pts',(-7.65741532450727,18.5788385228928,0.));
#15305=CARTESIAN_POINT('Ctrl Pts',(-7.65868976978872,18.6280491346907,0.));
#15306=CARTESIAN_POINT('Ctrl Pts',(-7.65962948375621,18.6773458057584,0.));
#15307=CARTESIAN_POINT('Ctrl Pts',(-7.66023521705904,18.7267272235231,0.));
#15308=CARTESIAN_POINT('Ctrl Pts',(-7.6605104692254,18.7761911671591,0.));
#15309=CARTESIAN_POINT('Ctrl Pts',(-7.66046025294774,18.8257349246207,0.));
#15310=CARTESIAN_POINT('Ctrl Pts',(-7.66009036321663,18.8753555389435,0.));
#15311=CARTESIAN_POINT('Ctrl Pts',(-7.65940650980098,18.9250501008887,0.));
#15312=CARTESIAN_POINT('Ctrl Pts',(-7.65841335587266,18.974816073814,0.));
#15313=CARTESIAN_POINT('Ctrl Pts',(-7.65711415727855,19.0246514144531,0.));
#15314=CARTESIAN_POINT('Ctrl Pts',(-7.65551129907201,19.0745543888799,0.));
#15315=CARTESIAN_POINT('Ctrl Pts',(-7.65360662280609,19.1245234597312,0.));
#15316=CARTESIAN_POINT('Ctrl Pts',(-7.65140181220525,19.1745571539291,0.));
#15317=CARTESIAN_POINT('Ctrl Pts',(-7.64889882291923,19.224653915265,0.));
#15318=CARTESIAN_POINT('Ctrl Pts',(-7.64610005549613,19.2748120456486,0.));
#15319=CARTESIAN_POINT('Ctrl Pts',(-7.64300812875338,19.3250297839295,0.));
#15320=CARTESIAN_POINT('Ctrl Pts',(-7.6396257482276,19.3753053524647,0.));
#15321=CARTESIAN_POINT('Ctrl Pts',(-7.63595554930654,19.4256370121006,0.));
#15322=CARTESIAN_POINT('Ctrl Pts',(-7.63199992715365,19.4760231231881,0.));
#15323=CARTESIAN_POINT('Ctrl Pts',(-7.62776096538882,19.5264621687521,0.));
#15324=CARTESIAN_POINT('Ctrl Pts',(-7.62324053735219,19.5769527121826,0.));
#15325=CARTESIAN_POINT('Ctrl Pts',(-7.6184403707059,19.6274933688524,0.));
#15326=CARTESIAN_POINT('Ctrl Pts',(-7.61336212350879,19.6780827744426,0.));
#15327=CARTESIAN_POINT('Ctrl Pts',(-7.60800746969261,19.7287195480601,0.));
#15328=CARTESIAN_POINT('Ctrl Pts',(-7.60237814110186,19.7794022782484,0.));
#15329=CARTESIAN_POINT('Ctrl Pts',(-7.59647587605448,19.830129556152,0.));
#15330=CARTESIAN_POINT('Ctrl Pts',(-7.59030238888852,19.8808999994024,0.));
#15331=CARTESIAN_POINT('Ctrl Pts',(-7.58385933533351,19.931712276832,0.));
#15332=CARTESIAN_POINT('Ctrl Pts',(-7.57714827622806,19.9825651387294,0.));
#15333=CARTESIAN_POINT('Ctrl Pts',(-7.57017066105973,20.0334574248556,0.));
#15334=CARTESIAN_POINT('Ctrl Pts',(-7.5629278654946,20.0843880130978,0.));
#15335=CARTESIAN_POINT('Ctrl Pts',(-7.55542122125494,20.1353557774357,0.));
#15336=CARTESIAN_POINT('Ctrl Pts',(-7.54765204869254,20.1863595454674,0.));
#15337=CARTESIAN_POINT('Ctrl Pts',(-7.53962169534166,20.2373980474879,0.));
#15338=CARTESIAN_POINT('Ctrl Pts',(-7.53133155804007,20.2884698940944,0.));
#15339=CARTESIAN_POINT('Ctrl Pts',(-7.52278303006887,20.3395736743243,0.));
#15340=CARTESIAN_POINT('Ctrl Pts',(-7.51397746081993,20.3907080367098,0.));
#15341=CARTESIAN_POINT('Ctrl Pts',(-7.50491611266253,20.4418717748497,0.));
#15342=CARTESIAN_POINT('Ctrl Pts',(-7.49560012018405,20.4930639156161,0.));
#15343=CARTESIAN_POINT('Ctrl Pts',(-7.48411651832412,20.5545277683621,0.));
#15344=CARTESIAN_POINT('Ctrl Pts',(-7.47423073598681,20.6057817877246,0.));
#15345=CARTESIAN_POINT('Ctrl Pts',(-7.46612041736313,20.6468066077586,0.));
#15346=CARTESIAN_POINT('Ctrl Pts',(-7.45992433946823,20.6775873630604,0.));
#15347=CARTESIAN_POINT('Ctrl Pts',(-7.45574324794401,20.698113262342,0.));
#15348=CARTESIAN_POINT('',(-7.45574324794407,20.698113262342,13.));
#15349=CARTESIAN_POINT('Ctrl Pts',(-7.45574324794401,20.698113262342,13.));
#15350=CARTESIAN_POINT('Ctrl Pts',(-7.47632490128082,20.5970733922996,13.));
#15351=CARTESIAN_POINT('Ctrl Pts',(-7.49544541996018,20.4961877827456,13.));
#15352=CARTESIAN_POINT('Ctrl Pts',(-7.51308219880446,20.3954689810171,13.));
#15353=CARTESIAN_POINT('Ctrl Pts',(-7.54230710697449,20.2285735542786,13.));
#15354=CARTESIAN_POINT('Ctrl Pts',(-7.56745095717373,20.062147728883,13.));
#15355=CARTESIAN_POINT('Ctrl Pts',(-7.58830059932795,19.8963869101261,13.));
#15356=CARTESIAN_POINT('Ctrl Pts',(-7.60432685704092,19.7689734235799,13.));
#15357=CARTESIAN_POINT('Ctrl Pts',(-7.61781485448689,19.6419503916105,13.));
#15358=CARTESIAN_POINT('Ctrl Pts',(-7.62864367953763,19.5154161616707,13.));
#15359=CARTESIAN_POINT('Ctrl Pts',(-7.6403006489712,19.3792051097978,13.));
#15360=CARTESIAN_POINT('Ctrl Pts',(-7.64888186442765,19.2435576430979,13.));
#15361=CARTESIAN_POINT('Ctrl Pts',(-7.65417053744727,19.1086228829228,13.));
#15362=CARTESIAN_POINT('Ctrl Pts',(-7.6570984904302,19.0339193359104,13.));
#15363=CARTESIAN_POINT('Ctrl Pts',(-7.65902218172414,18.9594327317773,13.));
#15364=CARTESIAN_POINT('Ctrl Pts',(-7.65990167998771,18.8851905412181,13.));
#15365=CARTESIAN_POINT('Ctrl Pts',(-7.66074919903711,18.813647852193,13.));
#15366=CARTESIAN_POINT('Ctrl Pts',(-7.66062065571968,18.742334282715,13.));
#15367=CARTESIAN_POINT('Ctrl Pts',(-7.65944821270105,18.6712863090353,13.));
#15368=CARTESIAN_POINT('Ctrl Pts',(-7.65843486239238,18.6098790722535,13.));
#15369=CARTESIAN_POINT('Ctrl Pts',(-7.65664478982501,18.5486691992234,13.));
#15370=CARTESIAN_POINT('Ctrl Pts',(-7.65407864070033,18.4876659850186,13.));
#15371=CARTESIAN_POINT('Ctrl Pts',(-7.6522370315783,18.4438867382584,13.));
#15372=CARTESIAN_POINT('Ctrl Pts',(-7.64999840197637,18.4002130327903,13.));
#15373=CARTESIAN_POINT('Ctrl Pts',(-7.64732656562888,18.3566609384397,13.));
#15374=CARTESIAN_POINT('Ctrl Pts',(-7.64469823681671,18.3138180358347,13.));
#15375=CARTESIAN_POINT('Ctrl Pts',(-7.64164464440333,18.2710948573601,13.));
#15376=CARTESIAN_POINT('Ctrl Pts',(-7.63811742044703,18.2285117408546,13.));
#15377=CARTESIAN_POINT('Ctrl Pts',(-7.63505911004952,18.1915896770503,13.));
#15378=CARTESIAN_POINT('Ctrl Pts',(-7.63164238136491,18.154773706468,13.));
#15379=CARTESIAN_POINT('Ctrl Pts',(-7.62788266166224,18.1180614604547,13.));
#15380=CARTESIAN_POINT('Ctrl Pts',(-7.62447721821964,18.0848085886088,13.));
#15381=CARTESIAN_POINT('Ctrl Pts',(-7.6207956490075,18.0516390296698,13.));
#15382=CARTESIAN_POINT('Ctrl Pts',(-7.61686093607981,18.0185473585012,13.));
#15383=CARTESIAN_POINT('Ctrl Pts',(-7.61354654175259,17.9906726827078,13.));
#15384=CARTESIAN_POINT('Ctrl Pts',(-7.6100541756254,17.9628527174308,13.));
#15385=CARTESIAN_POINT('Ctrl Pts',(-7.60636550501162,17.9350952313316,13.));
#15386=CARTESIAN_POINT('Ctrl Pts',(-7.60102759729446,17.8949271288438,13.));
#15387=CARTESIAN_POINT('Ctrl Pts',(-7.59527782596713,17.8548900767291,13.));
#15388=CARTESIAN_POINT('Ctrl Pts',(-7.58891067825601,17.8150590779502,13.));
#15389=CARTESIAN_POINT('Ctrl Pts',(-7.58506340059149,17.7909916432194,13.));
#15390=CARTESIAN_POINT('Ctrl Pts',(-7.58098742039303,17.7670005717874,13.));
#15391=CARTESIAN_POINT('Ctrl Pts',(-7.5766581762109,17.7430955913527,13.));
#15392=CARTESIAN_POINT('Ctrl Pts',(-7.57266539518276,17.7210484745022,13.));
#15393=CARTESIAN_POINT('Ctrl Pts',(-7.56845593268005,17.6990750118723,13.));
#15394=CARTESIAN_POINT('Ctrl Pts',(-7.56405390354134,17.677168309438,13.));
#15395=CARTESIAN_POINT('Ctrl Pts',(-7.5579984663457,17.6470334201461,13.));
#15396=CARTESIAN_POINT('Ctrl Pts',(-7.5515855270709,17.617022406593,13.));
#15397=CARTESIAN_POINT('Ctrl Pts',(-7.54495919885966,17.5870909089508,13.));
#15398=CARTESIAN_POINT('Ctrl Pts',(-7.54075533804246,17.5681018329307,13.));
#15399=CARTESIAN_POINT('Ctrl Pts',(-7.53646718585994,17.5491442491042,13.));
#15400=CARTESIAN_POINT('Ctrl Pts',(-7.53210330803509,17.5302169633315,13.));
#15401=CARTESIAN_POINT('Ctrl Pts',(-7.52818693080709,17.5132306053344,13.));
#15402=CARTESIAN_POINT('Ctrl Pts',(-7.5242102522165,17.4962684161094,13.));
#15403=CARTESIAN_POINT('Ctrl Pts',(-7.52014106530733,17.4793429835295,13.));
#15404=CARTESIAN_POINT('Ctrl Pts',(-7.51586353943748,17.4615509829812,13.));
#15405=CARTESIAN_POINT('Ctrl Pts',(-7.51148394209978,17.4437995539472,13.));
#15406=CARTESIAN_POINT('Ctrl Pts',(-7.50690601561094,17.4261238143268,13.));
#15407=CARTESIAN_POINT('Ctrl Pts',(-7.4993020898442,17.3967644499347,13.));
#15408=CARTESIAN_POINT('Ctrl Pts',(-7.49114308214025,17.3676168188904,13.));
#15409=CARTESIAN_POINT('Ctrl Pts',(-7.4818397562212,17.3388922514977,13.));
#15410=CARTESIAN_POINT('Ctrl Pts',(-7.47670957121237,17.3230525027557,13.));
#15411=CARTESIAN_POINT('Ctrl Pts',(-7.47123011545034,17.3073418194582,13.));
#15412=CARTESIAN_POINT('Ctrl Pts',(-7.46532888197675,17.2917860605643,13.));
#15413=CARTESIAN_POINT('Ctrl Pts',(-7.46052853290803,17.279132253008,13.));
#15414=CARTESIAN_POINT('Ctrl Pts',(-7.45544915949044,17.2665809316753,13.));
#15415=CARTESIAN_POINT('Ctrl Pts',(-7.45007618140238,17.2541372868972,13.));
#15416=CARTESIAN_POINT('',(-7.45574324794407,20.698113262342,0.));
#15417=CARTESIAN_POINT('Origin',(-1.75106900012182E-12,5.38923623413286E-12,
0.));
#15418=CARTESIAN_POINT('',(-6.1342227326009,21.1275013067528,0.));
#15419=CARTESIAN_POINT('Origin',(-1.75106900012182E-12,5.38923623413286E-12,
0.));
#15420=CARTESIAN_POINT('',(-6.1342227326009,21.1275013067528,13.));
#15421=CARTESIAN_POINT('Origin',(-1.75106900012182E-12,5.38923623413286E-12,
13.));
#15422=CARTESIAN_POINT('',(-6.1342227326009,21.1275013067528,0.));
#15423=CARTESIAN_POINT('Ctrl Pts',(-4.1144891981253,18.337935196262,0.));
#15424=CARTESIAN_POINT('Ctrl Pts',(-4.1144891981253,18.337935196262,21.));
#15425=CARTESIAN_POINT('Ctrl Pts',(-4.11655269114951,18.3471320125699,0.));
#15426=CARTESIAN_POINT('Ctrl Pts',(-4.11655269114951,18.3471320125699,21.));
#15427=CARTESIAN_POINT('Ctrl Pts',(-4.12092019868859,18.3654573320481,0.));
#15428=CARTESIAN_POINT('Ctrl Pts',(-4.12092019868859,18.3654573320481,21.));
#15429=CARTESIAN_POINT('Ctrl Pts',(-4.12819301671078,18.3927403741815,0.));
#15430=CARTESIAN_POINT('Ctrl Pts',(-4.12819301671078,18.3927403741815,21.));
#15431=CARTESIAN_POINT('Ctrl Pts',(-4.13926275457062,18.4287286547442,0.));
#15432=CARTESIAN_POINT('Ctrl Pts',(-4.13926275457062,18.4287286547442,21.));
#15433=CARTESIAN_POINT('Ctrl Pts',(-4.15497867673974,18.4731856794913,0.));
#15434=CARTESIAN_POINT('Ctrl Pts',(-4.15497867673974,18.4731856794913,21.));
#15435=CARTESIAN_POINT('Ctrl Pts',(-4.17205262766561,18.5172668097744,0.));
#15436=CARTESIAN_POINT('Ctrl Pts',(-4.17205262766561,18.5172668097744,21.));
#15437=CARTESIAN_POINT('Ctrl Pts',(-4.1899696727862,18.5611217636409,0.));
#15438=CARTESIAN_POINT('Ctrl Pts',(-4.1899696727862,18.5611217636409,21.));
#15439=CARTESIAN_POINT('Ctrl Pts',(-4.20834600700664,18.6048602364653,0.));
#15440=CARTESIAN_POINT('Ctrl Pts',(-4.20834600700664,18.6048602364653,21.));
#15441=CARTESIAN_POINT('Ctrl Pts',(-4.22703266508918,18.6485210883348,0.));
#15442=CARTESIAN_POINT('Ctrl Pts',(-4.22703266508918,18.6485210883348,21.));
#15443=CARTESIAN_POINT('Ctrl Pts',(-4.24603817988452,18.6920958920047,0.));
#15444=CARTESIAN_POINT('Ctrl Pts',(-4.24603817988452,18.6920958920047,21.));
#15445=CARTESIAN_POINT('Ctrl Pts',(-4.26546636161932,18.735547949685,0.));
#15446=CARTESIAN_POINT('Ctrl Pts',(-4.26546636161932,18.735547949685,21.));
#15447=CARTESIAN_POINT('Ctrl Pts',(-4.28545098663153,18.778832216358,0.));
#15448=CARTESIAN_POINT('Ctrl Pts',(-4.28545098663153,18.778832216358,21.));
#15449=CARTESIAN_POINT('Ctrl Pts',(-4.30608591031525,18.8219166495975,0.));
#15450=CARTESIAN_POINT('Ctrl Pts',(-4.30608591031525,18.8219166495975,21.));
#15451=CARTESIAN_POINT('Ctrl Pts',(-4.32737526247704,18.8647973781745,0.));
#15452=CARTESIAN_POINT('Ctrl Pts',(-4.32737526247704,18.8647973781745,21.));
#15453=CARTESIAN_POINT('Ctrl Pts',(-4.34926881342021,18.9074876952706,0.));
#15454=CARTESIAN_POINT('Ctrl Pts',(-4.34926881342021,18.9074876952706,21.));
#15455=CARTESIAN_POINT('Ctrl Pts',(-4.37168516143122,18.9500107909187,0.));
#15456=CARTESIAN_POINT('Ctrl Pts',(-4.37168516143122,18.9500107909187,21.));
#15457=CARTESIAN_POINT('Ctrl Pts',(-4.39453820875554,18.9923914823906,0.));
#15458=CARTESIAN_POINT('Ctrl Pts',(-4.39453820875554,18.9923914823906,21.));
#15459=CARTESIAN_POINT('Ctrl Pts',(-4.41776558033331,19.034647328575,0.));
#15460=CARTESIAN_POINT('Ctrl Pts',(-4.41776558033331,19.034647328575,21.));
#15461=CARTESIAN_POINT('Ctrl Pts',(-4.44134542994081,19.0767833717249,0.));
#15462=CARTESIAN_POINT('Ctrl Pts',(-4.44134542994081,19.0767833717249,21.));
#15463=CARTESIAN_POINT('Ctrl Pts',(-4.46528051067021,19.1187970904932,0.));
#15464=CARTESIAN_POINT('Ctrl Pts',(-4.46528051067021,19.1187970904932,21.));
#15465=CARTESIAN_POINT('Ctrl Pts',(-4.48958819710576,19.1606814968494,0.));
#15466=CARTESIAN_POINT('Ctrl Pts',(-4.48958819710576,19.1606814968494,21.));
#15467=CARTESIAN_POINT('Ctrl Pts',(-4.51428889122954,19.2024287376926,0.));
#15468=CARTESIAN_POINT('Ctrl Pts',(-4.51428889122954,19.2024287376926,21.));
#15469=CARTESIAN_POINT('Ctrl Pts',(-4.53939338835151,19.2440340196551,0.));
#15470=CARTESIAN_POINT('Ctrl Pts',(-4.53939338835151,19.2440340196551,21.));
#15471=CARTESIAN_POINT('Ctrl Pts',(-4.5648965160674,19.2854975819105,0.));
#15472=CARTESIAN_POINT('Ctrl Pts',(-4.5648965160674,19.2854975819105,21.));
#15473=CARTESIAN_POINT('Ctrl Pts',(-4.59078395765677,19.3268225655679,0.));
#15474=CARTESIAN_POINT('Ctrl Pts',(-4.59078395765677,19.3268225655679,21.));
#15475=CARTESIAN_POINT('Ctrl Pts',(-4.61703633725712,19.3680137353983,0.));
#15476=CARTESIAN_POINT('Ctrl Pts',(-4.61703633725712,19.3680137353983,21.));
#15477=CARTESIAN_POINT('Ctrl Pts',(-4.64363405547472,19.4090759683639,0.));
#15478=CARTESIAN_POINT('Ctrl Pts',(-4.64363405547472,19.4090759683639,21.));
#15479=CARTESIAN_POINT('Ctrl Pts',(-4.67056260851453,19.4500125912299,0.));
#15480=CARTESIAN_POINT('Ctrl Pts',(-4.67056260851453,19.4500125912299,21.));
#15481=CARTESIAN_POINT('Ctrl Pts',(-4.69781487613784,19.4908246636763,0.));
#15482=CARTESIAN_POINT('Ctrl Pts',(-4.69781487613784,19.4908246636763,21.));
#15483=CARTESIAN_POINT('Ctrl Pts',(-4.72538815796615,19.531511899192,0.));
#15484=CARTESIAN_POINT('Ctrl Pts',(-4.72538815796615,19.531511899192,21.));
#15485=CARTESIAN_POINT('Ctrl Pts',(-4.7532823819461,19.5720732205813,0.));
#15486=CARTESIAN_POINT('Ctrl Pts',(-4.7532823819461,19.5720732205813,21.));
#15487=CARTESIAN_POINT('Ctrl Pts',(-4.7814979936173,19.6125074152527,0.));
#15488=CARTESIAN_POINT('Ctrl Pts',(-4.7814979936173,19.6125074152527,21.));
#15489=CARTESIAN_POINT('Ctrl Pts',(-4.8100336141806,19.6528138625329,0.));
#15490=CARTESIAN_POINT('Ctrl Pts',(-4.8100336141806,19.6528138625329,21.));
#15491=CARTESIAN_POINT('Ctrl Pts',(-4.83888510708974,19.6929928227072,0.));
#15492=CARTESIAN_POINT('Ctrl Pts',(-4.83888510708974,19.6929928227072,21.));
#15493=CARTESIAN_POINT('Ctrl Pts',(-4.86804682289086,19.7330450480715,0.));
#15494=CARTESIAN_POINT('Ctrl Pts',(-4.86804682289086,19.7330450480715,21.));
#15495=CARTESIAN_POINT('Ctrl Pts',(-4.89751233527804,19.772971552601,0.));
#15496=CARTESIAN_POINT('Ctrl Pts',(-4.89751233527804,19.772971552601,21.));
#15497=CARTESIAN_POINT('Ctrl Pts',(-4.92727531494346,19.8127733387903,0.));
#15498=CARTESIAN_POINT('Ctrl Pts',(-4.92727531494346,19.8127733387903,21.));
#15499=CARTESIAN_POINT('Ctrl Pts',(-4.95733049830096,19.8524510953961,0.));
#15500=CARTESIAN_POINT('Ctrl Pts',(-4.95733049830096,19.8524510953961,21.));
#15501=CARTESIAN_POINT('Ctrl Pts',(-4.98767405031333,19.8920050831202,0.));
#15502=CARTESIAN_POINT('Ctrl Pts',(-4.98767405031333,19.8920050831202,21.));
#15503=CARTESIAN_POINT('Ctrl Pts',(-5.01830302225557,19.931435301086,0.));
#15504=CARTESIAN_POINT('Ctrl Pts',(-5.01830302225557,19.931435301086,21.));
#15505=CARTESIAN_POINT('Ctrl Pts',(-5.04921502064063,19.9707415879783,0.));
#15506=CARTESIAN_POINT('Ctrl Pts',(-5.04921502064063,19.9707415879783,21.));
#15507=CARTESIAN_POINT('Ctrl Pts',(-5.08040781745336,20.0099237417205,0.));
#15508=CARTESIAN_POINT('Ctrl Pts',(-5.08040781745336,20.0099237417205,21.));
#15509=CARTESIAN_POINT('Ctrl Pts',(-5.11187891582334,20.0489816528155,0.));
#15510=CARTESIAN_POINT('Ctrl Pts',(-5.11187891582334,20.0489816528155,21.));
#15511=CARTESIAN_POINT('Ctrl Pts',(-5.14362537555397,20.087915358486,0.));
#15512=CARTESIAN_POINT('Ctrl Pts',(-5.14362537555397,20.087915358486,21.));
#15513=CARTESIAN_POINT('Ctrl Pts',(-5.17564404279921,20.1267249732337,0.));
#15514=CARTESIAN_POINT('Ctrl Pts',(-5.17564404279921,20.1267249732337,21.));
#15515=CARTESIAN_POINT('Ctrl Pts',(-5.20793168386163,20.1654106491899,0.));
#15516=CARTESIAN_POINT('Ctrl Pts',(-5.20793168386163,20.1654106491899,21.));
#15517=CARTESIAN_POINT('Ctrl Pts',(-5.2404851444189,20.2039725283917,0.));
#15518=CARTESIAN_POINT('Ctrl Pts',(-5.2404851444189,20.2039725283917,21.));
#15519=CARTESIAN_POINT('Ctrl Pts',(-5.2733015229815,20.2424106921768,0.));
#15520=CARTESIAN_POINT('Ctrl Pts',(-5.2733015229815,20.2424106921768,21.));
#15521=CARTESIAN_POINT('Ctrl Pts',(-5.30637824220997,20.2807251380077,0.));
#15522=CARTESIAN_POINT('Ctrl Pts',(-5.30637824220997,20.2807251380077,21.));
#15523=CARTESIAN_POINT('Ctrl Pts',(-5.33971294212213,20.3189158047642,0.));
#15524=CARTESIAN_POINT('Ctrl Pts',(-5.33971294212213,20.3189158047642,21.));
#15525=CARTESIAN_POINT('Ctrl Pts',(-5.37330341114649,20.3569825877537,0.));
#15526=CARTESIAN_POINT('Ctrl Pts',(-5.37330341114649,20.3569825877537,21.));
#15527=CARTESIAN_POINT('Ctrl Pts',(-5.40714750595875,20.3949253578015,0.));
#15528=CARTESIAN_POINT('Ctrl Pts',(-5.40714750595875,20.3949253578015,21.));
#15529=CARTESIAN_POINT('Ctrl Pts',(-5.44124306065111,20.4327439816542,0.));
#15530=CARTESIAN_POINT('Ctrl Pts',(-5.44124306065111,20.4327439816542,21.));
#15531=CARTESIAN_POINT('Ctrl Pts',(-5.4755878444985,20.4704383353718,0.));
#15532=CARTESIAN_POINT('Ctrl Pts',(-5.4755878444985,20.4704383353718,21.));
#15533=CARTESIAN_POINT('Ctrl Pts',(-5.51017962306782,20.5080083009242,0.));
#15534=CARTESIAN_POINT('Ctrl Pts',(-5.51017962306782,20.5080083009242,21.));
#15535=CARTESIAN_POINT('Ctrl Pts',(-5.5450161968946,20.5454537676144,0.));
#15536=CARTESIAN_POINT('Ctrl Pts',(-5.5450161968946,20.5454537676144,21.));
#15537=CARTESIAN_POINT('Ctrl Pts',(-5.58009544402475,20.5827746317185,0.));
#15538=CARTESIAN_POINT('Ctrl Pts',(-5.58009544402475,20.5827746317185,21.));
#15539=CARTESIAN_POINT('Ctrl Pts',(-5.61541536715149,20.6199707996366,0.));
#15540=CARTESIAN_POINT('Ctrl Pts',(-5.61541536715149,20.6199707996366,21.));
#15541=CARTESIAN_POINT('Ctrl Pts',(-5.65097411164334,20.6570421847033,0.));
#15542=CARTESIAN_POINT('Ctrl Pts',(-5.65097411164334,20.6570421847033,21.));
#15543=CARTESIAN_POINT('Ctrl Pts',(-5.68676990500163,20.6939886877061,0.));
#15544=CARTESIAN_POINT('Ctrl Pts',(-5.68676990500163,20.6939886877061,21.));
#15545=CARTESIAN_POINT('Ctrl Pts',(-5.72280100798241,20.7308101804425,0.));
#15546=CARTESIAN_POINT('Ctrl Pts',(-5.72280100798241,20.7308101804425,21.));
#15547=CARTESIAN_POINT('Ctrl Pts',(-5.75906566327796,20.7675064905026,0.));
#15548=CARTESIAN_POINT('Ctrl Pts',(-5.75906566327796,20.7675064905026,21.));
#15549=CARTESIAN_POINT('Ctrl Pts',(-5.79556203439644,20.8040773827343,0.));
#15550=CARTESIAN_POINT('Ctrl Pts',(-5.79556203439644,20.8040773827343,21.));
#15551=CARTESIAN_POINT('Ctrl Pts',(-5.83228817460177,20.8405225541277,0.));
#15552=CARTESIAN_POINT('Ctrl Pts',(-5.83228817460177,20.8405225541277,21.));
#15553=CARTESIAN_POINT('Ctrl Pts',(-5.86924212736287,20.8768416821402,0.));
#15554=CARTESIAN_POINT('Ctrl Pts',(-5.86924212736287,20.8768416821402,21.));
#15555=CARTESIAN_POINT('Ctrl Pts',(-5.90642200662599,20.9130344665641,0.));
#15556=CARTESIAN_POINT('Ctrl Pts',(-5.90642200662599,20.9130344665641,21.));
#15557=CARTESIAN_POINT('Ctrl Pts',(-5.94382608200804,20.9491006734021,0.));
#15558=CARTESIAN_POINT('Ctrl Pts',(-5.94382608200804,20.9491006734021,21.));
#15559=CARTESIAN_POINT('Ctrl Pts',(-5.98145286361836,20.9850401822713,0.));
#15560=CARTESIAN_POINT('Ctrl Pts',(-5.98145286361836,20.9850401822713,21.));
#15561=CARTESIAN_POINT('Ctrl Pts',(-6.01930117633044,21.0208530236003,0.));
#15562=CARTESIAN_POINT('Ctrl Pts',(-6.01930117633044,21.0208530236003,21.));
#15563=CARTESIAN_POINT('Ctrl Pts',(-6.05737013696532,21.0565393163693,0.));
#15564=CARTESIAN_POINT('Ctrl Pts',(-6.05737013696532,21.0565393163693,21.));
#15565=CARTESIAN_POINT('Ctrl Pts',(-6.08800133883114,21.0849872356853,0.));
#15566=CARTESIAN_POINT('Ctrl Pts',(-6.08800133883114,21.0849872356853,21.));
#15567=CARTESIAN_POINT('Ctrl Pts',(-6.11107360216958,21.1062663590356,0.));
#15568=CARTESIAN_POINT('Ctrl Pts',(-6.11107360216958,21.1062663590356,21.));
#15569=CARTESIAN_POINT('Ctrl Pts',(-6.12649903511517,21.1204271980506,0.));
#15570=CARTESIAN_POINT('Ctrl Pts',(-6.12649903511517,21.1204271980506,21.));
#15571=CARTESIAN_POINT('Ctrl Pts',(-6.1342227326009,21.1275013067528,0.));
#15572=CARTESIAN_POINT('Ctrl Pts',(-6.1342227326009,21.1275013067528,21.));
#15573=CARTESIAN_POINT('Ctrl Pts',(-4.1144891981253,18.337935196262,0.));
#15574=CARTESIAN_POINT('Ctrl Pts',(-4.11655269114951,18.3471320125699,0.));
#15575=CARTESIAN_POINT('Ctrl Pts',(-4.12092019868859,18.3654573320481,0.));
#15576=CARTESIAN_POINT('Ctrl Pts',(-4.12819301671078,18.3927403741815,0.));
#15577=CARTESIAN_POINT('Ctrl Pts',(-4.13926275457062,18.4287286547442,0.));
#15578=CARTESIAN_POINT('Ctrl Pts',(-4.15497867673974,18.4731856794913,0.));
#15579=CARTESIAN_POINT('Ctrl Pts',(-4.17205262766561,18.5172668097744,0.));
#15580=CARTESIAN_POINT('Ctrl Pts',(-4.1899696727862,18.5611217636409,0.));
#15581=CARTESIAN_POINT('Ctrl Pts',(-4.20834600700664,18.6048602364653,0.));
#15582=CARTESIAN_POINT('Ctrl Pts',(-4.22703266508918,18.6485210883348,0.));
#15583=CARTESIAN_POINT('Ctrl Pts',(-4.24603817988452,18.6920958920047,0.));
#15584=CARTESIAN_POINT('Ctrl Pts',(-4.26546636161932,18.735547949685,0.));
#15585=CARTESIAN_POINT('Ctrl Pts',(-4.28545098663153,18.778832216358,0.));
#15586=CARTESIAN_POINT('Ctrl Pts',(-4.30608591031525,18.8219166495975,0.));
#15587=CARTESIAN_POINT('Ctrl Pts',(-4.32737526247704,18.8647973781745,0.));
#15588=CARTESIAN_POINT('Ctrl Pts',(-4.34926881342021,18.9074876952706,0.));
#15589=CARTESIAN_POINT('Ctrl Pts',(-4.37168516143122,18.9500107909187,0.));
#15590=CARTESIAN_POINT('Ctrl Pts',(-4.39453820875554,18.9923914823906,0.));
#15591=CARTESIAN_POINT('Ctrl Pts',(-4.41776558033331,19.034647328575,0.));
#15592=CARTESIAN_POINT('Ctrl Pts',(-4.44134542994081,19.0767833717249,0.));
#15593=CARTESIAN_POINT('Ctrl Pts',(-4.46528051067021,19.1187970904932,0.));
#15594=CARTESIAN_POINT('Ctrl Pts',(-4.48958819710576,19.1606814968494,0.));
#15595=CARTESIAN_POINT('Ctrl Pts',(-4.51428889122954,19.2024287376926,0.));
#15596=CARTESIAN_POINT('Ctrl Pts',(-4.53939338835151,19.2440340196551,0.));
#15597=CARTESIAN_POINT('Ctrl Pts',(-4.5648965160674,19.2854975819105,0.));
#15598=CARTESIAN_POINT('Ctrl Pts',(-4.59078395765677,19.3268225655679,0.));
#15599=CARTESIAN_POINT('Ctrl Pts',(-4.61703633725712,19.3680137353983,0.));
#15600=CARTESIAN_POINT('Ctrl Pts',(-4.64363405547472,19.4090759683639,0.));
#15601=CARTESIAN_POINT('Ctrl Pts',(-4.67056260851453,19.4500125912299,0.));
#15602=CARTESIAN_POINT('Ctrl Pts',(-4.69781487613784,19.4908246636763,0.));
#15603=CARTESIAN_POINT('Ctrl Pts',(-4.72538815796615,19.531511899192,0.));
#15604=CARTESIAN_POINT('Ctrl Pts',(-4.7532823819461,19.5720732205813,0.));
#15605=CARTESIAN_POINT('Ctrl Pts',(-4.7814979936173,19.6125074152527,0.));
#15606=CARTESIAN_POINT('Ctrl Pts',(-4.8100336141806,19.6528138625329,0.));
#15607=CARTESIAN_POINT('Ctrl Pts',(-4.83888510708974,19.6929928227072,0.));
#15608=CARTESIAN_POINT('Ctrl Pts',(-4.86804682289086,19.7330450480715,0.));
#15609=CARTESIAN_POINT('Ctrl Pts',(-4.89751233527804,19.772971552601,0.));
#15610=CARTESIAN_POINT('Ctrl Pts',(-4.92727531494346,19.8127733387903,0.));
#15611=CARTESIAN_POINT('Ctrl Pts',(-4.95733049830096,19.8524510953961,0.));
#15612=CARTESIAN_POINT('Ctrl Pts',(-4.98767405031333,19.8920050831202,0.));
#15613=CARTESIAN_POINT('Ctrl Pts',(-5.01830302225557,19.931435301086,0.));
#15614=CARTESIAN_POINT('Ctrl Pts',(-5.04921502064063,19.9707415879783,0.));
#15615=CARTESIAN_POINT('Ctrl Pts',(-5.08040781745336,20.0099237417205,0.));
#15616=CARTESIAN_POINT('Ctrl Pts',(-5.11187891582334,20.0489816528155,0.));
#15617=CARTESIAN_POINT('Ctrl Pts',(-5.14362537555397,20.087915358486,0.));
#15618=CARTESIAN_POINT('Ctrl Pts',(-5.17564404279921,20.1267249732337,0.));
#15619=CARTESIAN_POINT('Ctrl Pts',(-5.20793168386163,20.1654106491899,0.));
#15620=CARTESIAN_POINT('Ctrl Pts',(-5.2404851444189,20.2039725283917,0.));
#15621=CARTESIAN_POINT('Ctrl Pts',(-5.2733015229815,20.2424106921768,0.));
#15622=CARTESIAN_POINT('Ctrl Pts',(-5.30637824220997,20.2807251380077,0.));
#15623=CARTESIAN_POINT('Ctrl Pts',(-5.33971294212213,20.3189158047642,0.));
#15624=CARTESIAN_POINT('Ctrl Pts',(-5.37330341114649,20.3569825877537,0.));
#15625=CARTESIAN_POINT('Ctrl Pts',(-5.40714750595875,20.3949253578015,0.));
#15626=CARTESIAN_POINT('Ctrl Pts',(-5.44124306065111,20.4327439816542,0.));
#15627=CARTESIAN_POINT('Ctrl Pts',(-5.4755878444985,20.4704383353718,0.));
#15628=CARTESIAN_POINT('Ctrl Pts',(-5.51017962306782,20.5080083009242,0.));
#15629=CARTESIAN_POINT('Ctrl Pts',(-5.5450161968946,20.5454537676144,0.));
#15630=CARTESIAN_POINT('Ctrl Pts',(-5.58009544402475,20.5827746317185,0.));
#15631=CARTESIAN_POINT('Ctrl Pts',(-5.61541536715149,20.6199707996366,0.));
#15632=CARTESIAN_POINT('Ctrl Pts',(-5.65097411164334,20.6570421847033,0.));
#15633=CARTESIAN_POINT('Ctrl Pts',(-5.68676990500163,20.6939886877061,0.));
#15634=CARTESIAN_POINT('Ctrl Pts',(-5.72280100798241,20.7308101804425,0.));
#15635=CARTESIAN_POINT('Ctrl Pts',(-5.75906566327796,20.7675064905026,0.));
#15636=CARTESIAN_POINT('Ctrl Pts',(-5.79556203439644,20.8040773827343,0.));
#15637=CARTESIAN_POINT('Ctrl Pts',(-5.83228817460177,20.8405225541277,0.));
#15638=CARTESIAN_POINT('Ctrl Pts',(-5.86924212736287,20.8768416821402,0.));
#15639=CARTESIAN_POINT('Ctrl Pts',(-5.90642200662599,20.9130344665641,0.));
#15640=CARTESIAN_POINT('Ctrl Pts',(-5.94382608200804,20.9491006734021,0.));
#15641=CARTESIAN_POINT('Ctrl Pts',(-5.98145286361836,20.9850401822713,0.));
#15642=CARTESIAN_POINT('Ctrl Pts',(-6.02687083887286,21.0280155918661,0.));
#15643=CARTESIAN_POINT('Ctrl Pts',(-6.06499496148844,21.0636702474951,0.));
#15644=CARTESIAN_POINT('Ctrl Pts',(-6.09567013127871,21.0920928984154,0.));
#15645=CARTESIAN_POINT('Ctrl Pts',(-6.11877533761502,21.1133530893457,0.));
#15646=CARTESIAN_POINT('Ctrl Pts',(-6.1342227326009,21.1275013067528,0.));
#15647=CARTESIAN_POINT('Ctrl Pts',(-4.1144891981253,18.337935196262,13.));
#15648=CARTESIAN_POINT('Ctrl Pts',(-4.11796712887951,18.3534360435645,13.));
#15649=CARTESIAN_POINT('Ctrl Pts',(-4.12185943358937,18.3688191548995,13.));
#15650=CARTESIAN_POINT('Ctrl Pts',(-4.12613856044267,18.3840926404824,13.));
#15651=CARTESIAN_POINT('Ctrl Pts',(-4.13115401716693,18.4019943079477,13.));
#15652=CARTESIAN_POINT('Ctrl Pts',(-4.13670006307401,18.4197456248295,13.));
#15653=CARTESIAN_POINT('Ctrl Pts',(-4.1426637807957,18.4373797424196,13.));
#15654=CARTESIAN_POINT('Ctrl Pts',(-4.15105501703309,18.4621917897769,13.));
#15655=CARTESIAN_POINT('Ctrl Pts',(-4.16026629328986,18.4867739015683,13.));
#15656=CARTESIAN_POINT('Ctrl Pts',(-4.16990400115281,18.5112408492934,13.));
#15657=CARTESIAN_POINT('Ctrl Pts',(-4.17631459686345,18.5275152282609,13.));
#15658=CARTESIAN_POINT('Ctrl Pts',(-4.18291190640786,18.5437392096496,13.));
#15659=CARTESIAN_POINT('Ctrl Pts',(-4.18960898617042,18.5599376581358,13.));
#15660=CARTESIAN_POINT('Ctrl Pts',(-4.19665876042785,18.5769891804703,13.));
#15661=CARTESIAN_POINT('Ctrl Pts',(-4.20381824254442,18.5940126577989,13.));
#15662=CARTESIAN_POINT('Ctrl Pts',(-4.21104759333806,18.6110185062838,13.));
#15663=CARTESIAN_POINT('Ctrl Pts',(-4.21907618313382,18.6299044319376,13.));
#15664=CARTESIAN_POINT('Ctrl Pts',(-4.22719219297435,18.6487682283615,13.));
#15665=CARTESIAN_POINT('Ctrl Pts',(-4.23540730606871,18.6676042988365,13.));
#15666=CARTESIAN_POINT('Ctrl Pts',(-4.24779198778706,18.6960005893047,13.));
#15667=CARTESIAN_POINT('Ctrl Pts',(-4.26040793123126,18.7243319351566,13.));
#15668=CARTESIAN_POINT('Ctrl Pts',(-4.27340283281641,18.7525479285623,13.));
#15669=CARTESIAN_POINT('Ctrl Pts',(-4.28284334471974,18.7730462309053,13.));
#15670=CARTESIAN_POINT('Ctrl Pts',(-4.29248702330122,18.7934827312586,13.));
#15671=CARTESIAN_POINT('Ctrl Pts',(-4.30235320731447,18.8138501272238,13.));
#15672=CARTESIAN_POINT('Ctrl Pts',(-4.31441377244466,18.8387475247628,13.));
#15673=CARTESIAN_POINT('Ctrl Pts',(-4.32680560862846,18.8635420328974,13.));
#15674=CARTESIAN_POINT('Ctrl Pts',(-4.33948253068855,18.888246010372,13.));
#15675=CARTESIAN_POINT('Ctrl Pts',(-4.35317571045463,18.9149304060711,13.));
#15676=CARTESIAN_POINT('Ctrl Pts',(-4.36719580768566,18.9415109549159,13.));
#15677=CARTESIAN_POINT('Ctrl Pts',(-4.3814546652845,18.9680129070776,13.));
#15678=CARTESIAN_POINT('Ctrl Pts',(-4.39461837563789,18.9924793848188,13.));
#15679=CARTESIAN_POINT('Ctrl Pts',(-4.40798318218919,19.0168796293449,13.));
#15680=CARTESIAN_POINT('Ctrl Pts',(-4.42152146523478,19.0412206988196,13.));
#15681=CARTESIAN_POINT('Ctrl Pts',(-4.43991391787386,19.0742892914905,13.));
#15682=CARTESIAN_POINT('Ctrl Pts',(-4.45862842578007,19.1072480695063,13.));
#15683=CARTESIAN_POINT('Ctrl Pts',(-4.47769255661886,19.1400849916113,13.));
#15684=CARTESIAN_POINT('Ctrl Pts',(-4.49608903112579,19.1717719122214,13.));
#15685=CARTESIAN_POINT('Ctrl Pts',(-4.51481852740326,19.2033430482922,13.));
#15686=CARTESIAN_POINT('Ctrl Pts',(-4.53389559678128,19.2347910922226,13.));
#15687=CARTESIAN_POINT('Ctrl Pts',(-4.55981233004855,19.2775141410396,13.));
#15688=CARTESIAN_POINT('Ctrl Pts',(-4.58636743963562,19.3200109590135,13.));
#15689=CARTESIAN_POINT('Ctrl Pts',(-4.61347737159604,19.3623013141123,13.));
#15690=CARTESIAN_POINT('Ctrl Pts',(-4.63730641242961,19.3994736168679,13.));
#15691=CARTESIAN_POINT('Ctrl Pts',(-4.66155758363823,19.4364884570226,13.));
#15692=CARTESIAN_POINT('Ctrl Pts',(-4.68619912923096,19.4733518502478,13.));
#15693=CARTESIAN_POINT('Ctrl Pts',(-4.72252674998903,19.527697441676,13.));
#15694=CARTESIAN_POINT('Ctrl Pts',(-4.75971143888908,19.5817111524814,13.));
#15695=CARTESIAN_POINT('Ctrl Pts',(-4.79774570283441,19.6353839062314,13.));
#15696=CARTESIAN_POINT('Ctrl Pts',(-4.84574531506025,19.7031194451863,13.));
#15697=CARTESIAN_POINT('Ctrl Pts',(-4.895093042552,19.7703134645498,13.));
#15698=CARTESIAN_POINT('Ctrl Pts',(-4.94566457605319,19.836983801638,13.));
#15699=CARTESIAN_POINT('Ctrl Pts',(-5.01416761715498,19.9272939133872,13.));
#15700=CARTESIAN_POINT('Ctrl Pts',(-5.08492180300406,20.01664136013,13.));
#15701=CARTESIAN_POINT('Ctrl Pts',(-5.15778644827778,20.105022570296,13.));
#15702=CARTESIAN_POINT('Ctrl Pts',(-5.22274718768723,20.1838167336481,13.));
#15703=CARTESIAN_POINT('Ctrl Pts',(-5.28937724215395,20.2618454265211,13.));
#15704=CARTESIAN_POINT('Ctrl Pts',(-5.35757729622096,20.3391090329722,13.));
#15705=CARTESIAN_POINT('Ctrl Pts',(-5.454235527518,20.4486128104304,13.));
#15706=CARTESIAN_POINT('Ctrl Pts',(-5.55405241051352,20.5565772409248,13.));
#15707=CARTESIAN_POINT('Ctrl Pts',(-5.65680258430444,20.6629906948204,13.));
#15708=CARTESIAN_POINT('Ctrl Pts',(-5.73661648166364,20.7456501412575,13.));
#15709=CARTESIAN_POINT('Ctrl Pts',(-5.81820510861819,20.8273750324251,13.));
#15710=CARTESIAN_POINT('Ctrl Pts',(-5.90147459212854,20.908152214715,13.));
#15711=CARTESIAN_POINT('Ctrl Pts',(-5.97350898952772,20.9780305831708,13.));
#15712=CARTESIAN_POINT('Ctrl Pts',(-6.04679718411003,21.0471984364812,13.));
#15713=CARTESIAN_POINT('Ctrl Pts',(-6.12131239112586,21.1156584400056,13.));
#15714=CARTESIAN_POINT('Ctrl Pts',(-6.12561173959338,21.1196084177756,13.));
#15715=CARTESIAN_POINT('Ctrl Pts',(-6.12991518682867,21.1235560399827,13.));
#15716=CARTESIAN_POINT('Ctrl Pts',(-6.1342227326009,21.1275013067528,13.));
#15717=CARTESIAN_POINT('Ctrl Pts',(-0.69476445021958,21.9890268624765,0.));
#15718=CARTESIAN_POINT('Ctrl Pts',(-0.69476445021958,21.9890268624765,21.));
#15719=CARTESIAN_POINT('Ctrl Pts',(-0.699924103234222,21.9799122315157,
0.));
#15720=CARTESIAN_POINT('Ctrl Pts',(-0.699924103234222,21.9799122315157,
21.));
#15721=CARTESIAN_POINT('Ctrl Pts',(-0.710218621843556,21.9616777523685,
0.));
#15722=CARTESIAN_POINT('Ctrl Pts',(-0.710218621843556,21.9616777523685,
21.));
#15723=CARTESIAN_POINT('Ctrl Pts',(-0.725586037496635,21.9343103819749,
0.));
#15724=CARTESIAN_POINT('Ctrl Pts',(-0.725586037496635,21.9343103819749,
21.));
#15725=CARTESIAN_POINT('Ctrl Pts',(-0.745927151109821,21.8977892409997,
0.));
#15726=CARTESIAN_POINT('Ctrl Pts',(-0.745927151109821,21.8977892409997,
21.));
#15727=CARTESIAN_POINT('Ctrl Pts',(-0.77110521325833,21.8520856039249,0.));
#15728=CARTESIAN_POINT('Ctrl Pts',(-0.77110521325833,21.8520856039249,21.));
#15729=CARTESIAN_POINT('Ctrl Pts',(-0.796034321106412,21.8063297959755,
0.));
#15730=CARTESIAN_POINT('Ctrl Pts',(-0.796034321106412,21.8063297959755,
21.));
#15731=CARTESIAN_POINT('Ctrl Pts',(-0.820713597934077,21.7605219769118,
0.));
#15732=CARTESIAN_POINT('Ctrl Pts',(-0.820713597934077,21.7605219769118,
21.));
#15733=CARTESIAN_POINT('Ctrl Pts',(-0.845141916726557,21.7146624809285,
0.));
#15734=CARTESIAN_POINT('Ctrl Pts',(-0.845141916726557,21.7146624809285,
21.));
#15735=CARTESIAN_POINT('Ctrl Pts',(-0.869317897714099,21.6687518829182,
0.));
#15736=CARTESIAN_POINT('Ctrl Pts',(-0.869317897714099,21.6687518829182,
21.));
#15737=CARTESIAN_POINT('Ctrl Pts',(-0.893239967513673,21.6227909401433,
0.));
#15738=CARTESIAN_POINT('Ctrl Pts',(-0.893239967513673,21.6227909401433,
21.));
#15739=CARTESIAN_POINT('Ctrl Pts',(-0.916906425150853,21.5767805209408,
0.));
#15740=CARTESIAN_POINT('Ctrl Pts',(-0.916906425150853,21.5767805209408,
21.));
#15741=CARTESIAN_POINT('Ctrl Pts',(-0.940315509525149,21.5307215366685,
0.));
#15742=CARTESIAN_POINT('Ctrl Pts',(-0.940315509525149,21.5307215366685,
21.));
#15743=CARTESIAN_POINT('Ctrl Pts',(-0.963465462815771,21.4846148770804,
0.));
#15744=CARTESIAN_POINT('Ctrl Pts',(-0.963465462815771,21.4846148770804,
21.));
#15745=CARTESIAN_POINT('Ctrl Pts',(-0.986354611081133,21.4384613333266,
0.));
#15746=CARTESIAN_POINT('Ctrl Pts',(-0.986354611081133,21.4384613333266,
21.));
#15747=CARTESIAN_POINT('Ctrl Pts',(-1.00898133629988,21.3922616124166,0.));
#15748=CARTESIAN_POINT('Ctrl Pts',(-1.00898133629988,21.3922616124166,21.));
#15749=CARTESIAN_POINT('Ctrl Pts',(-1.03134402396953,21.3460163737343,0.));
#15750=CARTESIAN_POINT('Ctrl Pts',(-1.03134402396953,21.3460163737343,21.));
#15751=CARTESIAN_POINT('Ctrl Pts',(-1.05344101900192,21.2997262593683,0.));
#15752=CARTESIAN_POINT('Ctrl Pts',(-1.05344101900192,21.2997262593683,21.));
#15753=CARTESIAN_POINT('Ctrl Pts',(-1.07527058431887,21.2533919248553,0.));
#15754=CARTESIAN_POINT('Ctrl Pts',(-1.07527058431887,21.2533919248553,21.));
#15755=CARTESIAN_POINT('Ctrl Pts',(-1.09683084929266,21.2070140764156,0.));
#15756=CARTESIAN_POINT('Ctrl Pts',(-1.09683084929266,21.2070140764156,21.));
#15757=CARTESIAN_POINT('Ctrl Pts',(-1.11811982787746,21.1605934684164,0.));
#15758=CARTESIAN_POINT('Ctrl Pts',(-1.11811982787746,21.1605934684164,21.));
#15759=CARTESIAN_POINT('Ctrl Pts',(-1.13913546246555,21.1141308858087,0.));
#15760=CARTESIAN_POINT('Ctrl Pts',(-1.13913546246555,21.1141308858087,21.));
#15761=CARTESIAN_POINT('Ctrl Pts',(-1.15987566445807,21.0676271313238,0.));
#15762=CARTESIAN_POINT('Ctrl Pts',(-1.15987566445807,21.0676271313238,21.));
#15763=CARTESIAN_POINT('Ctrl Pts',(-1.18033835060894,21.0210830121673,0.));
#15764=CARTESIAN_POINT('Ctrl Pts',(-1.18033835060894,21.0210830121673,21.));
#15765=CARTESIAN_POINT('Ctrl Pts',(-1.20052150219503,20.9744993243732,0.));
#15766=CARTESIAN_POINT('Ctrl Pts',(-1.20052150219503,20.9744993243732,21.));
#15767=CARTESIAN_POINT('Ctrl Pts',(-1.22042312071096,20.9278768531175,0.));
#15768=CARTESIAN_POINT('Ctrl Pts',(-1.22042312071096,20.9278768531175,21.));
#15769=CARTESIAN_POINT('Ctrl Pts',(-1.24004113517905,20.881216381382,0.));
#15770=CARTESIAN_POINT('Ctrl Pts',(-1.24004113517905,20.881216381382,21.));
#15771=CARTESIAN_POINT('Ctrl Pts',(-1.25937332001005,20.83451869657,0.));
#15772=CARTESIAN_POINT('Ctrl Pts',(-1.25937332001005,20.83451869657,21.));
#15773=CARTESIAN_POINT('Ctrl Pts',(-1.27841722479262,20.7877845975367,0.));
#15774=CARTESIAN_POINT('Ctrl Pts',(-1.27841722479262,20.7877845975367,21.));
#15775=CARTESIAN_POINT('Ctrl Pts',(-1.29717006491149,20.7410149035348,0.));
#15776=CARTESIAN_POINT('Ctrl Pts',(-1.29717006491149,20.7410149035348,21.));
#15777=CARTESIAN_POINT('Ctrl Pts',(-1.31562879653596,20.694210454218,0.));
#15778=CARTESIAN_POINT('Ctrl Pts',(-1.31562879653596,20.694210454218,21.));
#15779=CARTESIAN_POINT('Ctrl Pts',(-1.3337902972259,20.6473721041685,0.));
#15780=CARTESIAN_POINT('Ctrl Pts',(-1.3337902972259,20.6473721041685,21.));
#15781=CARTESIAN_POINT('Ctrl Pts',(-1.35165153211253,20.6005007190809,0.));
#15782=CARTESIAN_POINT('Ctrl Pts',(-1.35165153211253,20.6005007190809,21.));
#15783=CARTESIAN_POINT('Ctrl Pts',(-1.36920969340018,20.5535971721246,0.));
#15784=CARTESIAN_POINT('Ctrl Pts',(-1.36920969340018,20.5535971721246,21.));
#15785=CARTESIAN_POINT('Ctrl Pts',(-1.38646244026049,20.5066623390132,0.));
#15786=CARTESIAN_POINT('Ctrl Pts',(-1.38646244026049,20.5066623390132,21.));
#15787=CARTESIAN_POINT('Ctrl Pts',(-1.40340771617024,20.4596971004275,0.));
#15788=CARTESIAN_POINT('Ctrl Pts',(-1.40340771617024,20.4596971004275,21.));
#15789=CARTESIAN_POINT('Ctrl Pts',(-1.4200432946371,20.4127023494155,0.));
#15790=CARTESIAN_POINT('Ctrl Pts',(-1.4200432946371,20.4127023494155,21.));
#15791=CARTESIAN_POINT('Ctrl Pts',(-1.43636637152782,20.3656789980171,0.));
#15792=CARTESIAN_POINT('Ctrl Pts',(-1.43636637152782,20.3656789980171,21.));
#15793=CARTESIAN_POINT('Ctrl Pts',(-1.45237321894403,20.3186279833818,0.));
#15794=CARTESIAN_POINT('Ctrl Pts',(-1.45237321894403,20.3186279833818,21.));
#15795=CARTESIAN_POINT('Ctrl Pts',(-1.46805861808021,20.2715502770004,0.));
#15796=CARTESIAN_POINT('Ctrl Pts',(-1.46805861808021,20.2715502770004,21.));
#15797=CARTESIAN_POINT('Ctrl Pts',(-1.48341623961913,20.224446881308,0.));
#15798=CARTESIAN_POINT('Ctrl Pts',(-1.48341623961913,20.224446881308,21.));
#15799=CARTESIAN_POINT('Ctrl Pts',(-1.49843965844502,20.1773188177942,0.));
#15800=CARTESIAN_POINT('Ctrl Pts',(-1.49843965844502,20.1773188177942,21.));
#15801=CARTESIAN_POINT('Ctrl Pts',(-1.51312326913583,20.1301671167606,0.));
#15802=CARTESIAN_POINT('Ctrl Pts',(-1.51312326913583,20.1301671167606,21.));
#15803=CARTESIAN_POINT('Ctrl Pts',(-1.52746305716964,20.0829928089241,0.));
#15804=CARTESIAN_POINT('Ctrl Pts',(-1.52746305716964,20.0829928089241,21.));
#15805=CARTESIAN_POINT('Ctrl Pts',(-1.54145790302917,20.0357969106526,0.));
#15806=CARTESIAN_POINT('Ctrl Pts',(-1.54145790302917,20.0357969106526,21.));
#15807=CARTESIAN_POINT('Ctrl Pts',(-1.55510860515913,19.9885804375097,0.));
#15808=CARTESIAN_POINT('Ctrl Pts',(-1.55510860515913,19.9885804375097,21.));
#15809=CARTESIAN_POINT('Ctrl Pts',(-1.56841542790452,19.9413444362352,0.));
#15810=CARTESIAN_POINT('Ctrl Pts',(-1.56841542790452,19.9413444362352,21.));
#15811=CARTESIAN_POINT('Ctrl Pts',(-1.58137589158952,19.8940900137801,0.));
#15812=CARTESIAN_POINT('Ctrl Pts',(-1.58137589158952,19.8940900137801,21.));
#15813=CARTESIAN_POINT('Ctrl Pts',(-1.59398289700559,19.8468183626037,0.));
#15814=CARTESIAN_POINT('Ctrl Pts',(-1.59398289700559,19.8468183626037,21.));
#15815=CARTESIAN_POINT('Ctrl Pts',(-1.60622162219699,19.7995308006834,0.));
#15816=CARTESIAN_POINT('Ctrl Pts',(-1.60622162219699,19.7995308006834,21.));
#15817=CARTESIAN_POINT('Ctrl Pts',(-1.61807191996834,19.7522287462982,0.));
#15818=CARTESIAN_POINT('Ctrl Pts',(-1.61807191996834,19.7522287462982,21.));
#15819=CARTESIAN_POINT('Ctrl Pts',(-1.62951389038421,19.7049136553525,0.));
#15820=CARTESIAN_POINT('Ctrl Pts',(-1.62951389038421,19.7049136553525,21.));
#15821=CARTESIAN_POINT('Ctrl Pts',(-1.64053294677821,19.6575869645839,0.));
#15822=CARTESIAN_POINT('Ctrl Pts',(-1.64053294677821,19.6575869645839,21.));
#15823=CARTESIAN_POINT('Ctrl Pts',(-1.65112409599283,19.6102500448855,0.));
#15824=CARTESIAN_POINT('Ctrl Pts',(-1.65112409599283,19.6102500448855,21.));
#15825=CARTESIAN_POINT('Ctrl Pts',(-1.66129908621006,19.5629041190868,0.));
#15826=CARTESIAN_POINT('Ctrl Pts',(-1.66129908621006,19.5629041190868,21.));
#15827=CARTESIAN_POINT('Ctrl Pts',(-1.67107974760949,19.5155503513712,0.));
#15828=CARTESIAN_POINT('Ctrl Pts',(-1.67107974760949,19.5155503513712,21.));
#15829=CARTESIAN_POINT('Ctrl Pts',(-1.68048476382294,19.4681900187091,0.));
#15830=CARTESIAN_POINT('Ctrl Pts',(-1.68048476382294,19.4681900187091,21.));
#15831=CARTESIAN_POINT('Ctrl Pts',(-1.68951753233571,19.4208246682917,0.));
#15832=CARTESIAN_POINT('Ctrl Pts',(-1.68951753233571,19.4208246682917,21.));
#15833=CARTESIAN_POINT('Ctrl Pts',(-1.69815571801252,19.3734562555057,0.));
#15834=CARTESIAN_POINT('Ctrl Pts',(-1.69815571801252,19.3734562555057,21.));
#15835=CARTESIAN_POINT('Ctrl Pts',(-1.70633457265124,19.3260873558094,0.));
#15836=CARTESIAN_POINT('Ctrl Pts',(-1.70633457265124,19.3260873558094,21.));
#15837=CARTESIAN_POINT('Ctrl Pts',(-1.71396454346262,19.2787209722437,0.));
#15838=CARTESIAN_POINT('Ctrl Pts',(-1.71396454346262,19.2787209722437,21.));
#15839=CARTESIAN_POINT('Ctrl Pts',(-1.72096104670234,19.2313602042899,0.));
#15840=CARTESIAN_POINT('Ctrl Pts',(-1.72096104670234,19.2313602042899,21.));
#15841=CARTESIAN_POINT('Ctrl Pts',(-1.72727220327098,19.1840079312107,0.));
#15842=CARTESIAN_POINT('Ctrl Pts',(-1.72727220327098,19.1840079312107,21.));
#15843=CARTESIAN_POINT('Ctrl Pts',(-1.73290313712353,19.1366665585833,0.));
#15844=CARTESIAN_POINT('Ctrl Pts',(-1.73290313712353,19.1366665585833,21.));
#15845=CARTESIAN_POINT('Ctrl Pts',(-1.7379530116984,19.0893375576541,0.));
#15846=CARTESIAN_POINT('Ctrl Pts',(-1.7379530116984,19.0893375576541,21.));
#15847=CARTESIAN_POINT('Ctrl Pts',(-1.74256297552949,19.0420224296189,0.));
#15848=CARTESIAN_POINT('Ctrl Pts',(-1.74256297552949,19.0420224296189,21.));
#15849=CARTESIAN_POINT('Ctrl Pts',(-1.74684309825012,18.9947239970259,0.));
#15850=CARTESIAN_POINT('Ctrl Pts',(-1.74684309825012,18.9947239970259,21.));
#15851=CARTESIAN_POINT('Ctrl Pts',(-1.75080409924533,18.947447637865,0.));
#15852=CARTESIAN_POINT('Ctrl Pts',(-1.75080409924533,18.947447637865,21.));
#15853=CARTESIAN_POINT('Ctrl Pts',(-1.75429229572775,18.9002024267872,0.));
#15854=CARTESIAN_POINT('Ctrl Pts',(-1.75429229572775,18.9002024267872,21.));
#15855=CARTESIAN_POINT('Ctrl Pts',(-1.75690876962597,18.8530026395886,0.));
#15856=CARTESIAN_POINT('Ctrl Pts',(-1.75690876962597,18.8530026395886,21.));
#15857=CARTESIAN_POINT('Ctrl Pts',(-1.7581175236483,18.8058650094753,0.));
#15858=CARTESIAN_POINT('Ctrl Pts',(-1.7581175236483,18.8058650094753,21.));
#15859=CARTESIAN_POINT('Ctrl Pts',(-1.75752447968136,18.7682173836138,0.));
#15860=CARTESIAN_POINT('Ctrl Pts',(-1.75752447968136,18.7682173836138,21.));
#15861=CARTESIAN_POINT('Ctrl Pts',(-1.75601041697575,18.7400222442427,0.));
#15862=CARTESIAN_POINT('Ctrl Pts',(-1.75601041697575,18.7400222442427,21.));
#15863=CARTESIAN_POINT('Ctrl Pts',(-1.75450132833464,18.7212441956871,0.));
#15864=CARTESIAN_POINT('Ctrl Pts',(-1.75450132833464,18.7212441956871,21.));
#15865=CARTESIAN_POINT('Ctrl Pts',(-1.75362185428836,18.7118598491961,0.));
#15866=CARTESIAN_POINT('Ctrl Pts',(-1.75362185428836,18.7118598491961,21.));
#15867=CARTESIAN_POINT('',(-0.694764450219644,21.9890268624765,0.));
#15868=CARTESIAN_POINT('Ctrl Pts',(-1.75362185428836,18.7118598491961,0.));
#15869=CARTESIAN_POINT('Ctrl Pts',(-1.75450132833464,18.7212441956871,0.));
#15870=CARTESIAN_POINT('Ctrl Pts',(-1.75601041697575,18.7400222442427,0.));
#15871=CARTESIAN_POINT('Ctrl Pts',(-1.75752447968136,18.7682173836138,0.));
#15872=CARTESIAN_POINT('Ctrl Pts',(-1.7581175236483,18.8058650094753,0.));
#15873=CARTESIAN_POINT('Ctrl Pts',(-1.75690876962597,18.8530026395886,0.));
#15874=CARTESIAN_POINT('Ctrl Pts',(-1.75429229572775,18.9002024267872,0.));
#15875=CARTESIAN_POINT('Ctrl Pts',(-1.75080409924533,18.947447637865,0.));
#15876=CARTESIAN_POINT('Ctrl Pts',(-1.74684309825012,18.9947239970259,0.));
#15877=CARTESIAN_POINT('Ctrl Pts',(-1.74256297552949,19.0420224296189,0.));
#15878=CARTESIAN_POINT('Ctrl Pts',(-1.7379530116984,19.0893375576541,0.));
#15879=CARTESIAN_POINT('Ctrl Pts',(-1.73290313712353,19.1366665585833,0.));
#15880=CARTESIAN_POINT('Ctrl Pts',(-1.72727220327098,19.1840079312107,0.));
#15881=CARTESIAN_POINT('Ctrl Pts',(-1.72096104670234,19.2313602042899,0.));
#15882=CARTESIAN_POINT('Ctrl Pts',(-1.71396454346262,19.2787209722437,0.));
#15883=CARTESIAN_POINT('Ctrl Pts',(-1.70633457265124,19.3260873558094,0.));
#15884=CARTESIAN_POINT('Ctrl Pts',(-1.69815571801252,19.3734562555057,0.));
#15885=CARTESIAN_POINT('Ctrl Pts',(-1.68951753233571,19.4208246682917,0.));
#15886=CARTESIAN_POINT('Ctrl Pts',(-1.68048476382294,19.4681900187091,0.));
#15887=CARTESIAN_POINT('Ctrl Pts',(-1.67107974760949,19.5155503513712,0.));
#15888=CARTESIAN_POINT('Ctrl Pts',(-1.66129908621006,19.5629041190868,0.));
#15889=CARTESIAN_POINT('Ctrl Pts',(-1.65112409599283,19.6102500448855,0.));
#15890=CARTESIAN_POINT('Ctrl Pts',(-1.64053294677821,19.6575869645839,0.));
#15891=CARTESIAN_POINT('Ctrl Pts',(-1.62951389038421,19.7049136553525,0.));
#15892=CARTESIAN_POINT('Ctrl Pts',(-1.61807191996834,19.7522287462982,0.));
#15893=CARTESIAN_POINT('Ctrl Pts',(-1.60622162219699,19.7995308006834,0.));
#15894=CARTESIAN_POINT('Ctrl Pts',(-1.59398289700559,19.8468183626037,0.));
#15895=CARTESIAN_POINT('Ctrl Pts',(-1.58137589158952,19.8940900137801,0.));
#15896=CARTESIAN_POINT('Ctrl Pts',(-1.56841542790452,19.9413444362352,0.));
#15897=CARTESIAN_POINT('Ctrl Pts',(-1.55510860515913,19.9885804375097,0.));
#15898=CARTESIAN_POINT('Ctrl Pts',(-1.54145790302917,20.0357969106526,0.));
#15899=CARTESIAN_POINT('Ctrl Pts',(-1.52746305716964,20.0829928089241,0.));
#15900=CARTESIAN_POINT('Ctrl Pts',(-1.51312326913583,20.1301671167606,0.));
#15901=CARTESIAN_POINT('Ctrl Pts',(-1.49843965844502,20.1773188177942,0.));
#15902=CARTESIAN_POINT('Ctrl Pts',(-1.48341623961913,20.224446881308,0.));
#15903=CARTESIAN_POINT('Ctrl Pts',(-1.46805861808021,20.2715502770004,0.));
#15904=CARTESIAN_POINT('Ctrl Pts',(-1.45237321894403,20.3186279833818,0.));
#15905=CARTESIAN_POINT('Ctrl Pts',(-1.43636637152782,20.3656789980171,0.));
#15906=CARTESIAN_POINT('Ctrl Pts',(-1.4200432946371,20.4127023494155,0.));
#15907=CARTESIAN_POINT('Ctrl Pts',(-1.40340771617024,20.4596971004275,0.));
#15908=CARTESIAN_POINT('Ctrl Pts',(-1.38646244026049,20.5066623390132,0.));
#15909=CARTESIAN_POINT('Ctrl Pts',(-1.36920969340018,20.5535971721246,0.));
#15910=CARTESIAN_POINT('Ctrl Pts',(-1.35165153211253,20.6005007190809,0.));
#15911=CARTESIAN_POINT('Ctrl Pts',(-1.3337902972259,20.6473721041685,0.));
#15912=CARTESIAN_POINT('Ctrl Pts',(-1.31562879653596,20.694210454218,0.));
#15913=CARTESIAN_POINT('Ctrl Pts',(-1.29717006491149,20.7410149035348,0.));
#15914=CARTESIAN_POINT('Ctrl Pts',(-1.27841722479262,20.7877845975367,0.));
#15915=CARTESIAN_POINT('Ctrl Pts',(-1.25937332001005,20.83451869657,0.));
#15916=CARTESIAN_POINT('Ctrl Pts',(-1.24004113517905,20.881216381382,0.));
#15917=CARTESIAN_POINT('Ctrl Pts',(-1.22042312071096,20.9278768531175,0.));
#15918=CARTESIAN_POINT('Ctrl Pts',(-1.20052150219503,20.9744993243732,0.));
#15919=CARTESIAN_POINT('Ctrl Pts',(-1.18033835060894,21.0210830121673,0.));
#15920=CARTESIAN_POINT('Ctrl Pts',(-1.15987566445807,21.0676271313238,0.));
#15921=CARTESIAN_POINT('Ctrl Pts',(-1.13913546246555,21.1141308858087,0.));
#15922=CARTESIAN_POINT('Ctrl Pts',(-1.11811982787746,21.1605934684164,0.));
#15923=CARTESIAN_POINT('Ctrl Pts',(-1.09683084929266,21.2070140764156,0.));
#15924=CARTESIAN_POINT('Ctrl Pts',(-1.07527058431887,21.2533919248553,0.));
#15925=CARTESIAN_POINT('Ctrl Pts',(-1.05344101900192,21.2997262593683,0.));
#15926=CARTESIAN_POINT('Ctrl Pts',(-1.03134402396953,21.3460163737343,0.));
#15927=CARTESIAN_POINT('Ctrl Pts',(-1.00898133629988,21.3922616124166,0.));
#15928=CARTESIAN_POINT('Ctrl Pts',(-0.986354611081133,21.4384613333266,
0.));
#15929=CARTESIAN_POINT('Ctrl Pts',(-0.963465462815771,21.4846148770804,
0.));
#15930=CARTESIAN_POINT('Ctrl Pts',(-0.940315509525149,21.5307215366685,
0.));
#15931=CARTESIAN_POINT('Ctrl Pts',(-0.916906425150853,21.5767805209408,
0.));
#15932=CARTESIAN_POINT('Ctrl Pts',(-0.893239967513673,21.6227909401433,
0.));
#15933=CARTESIAN_POINT('Ctrl Pts',(-0.869317897714099,21.6687518829182,
0.));
#15934=CARTESIAN_POINT('Ctrl Pts',(-0.845141916726557,21.7146624809285,
0.));
#15935=CARTESIAN_POINT('Ctrl Pts',(-0.820713597934077,21.7605219769118,
0.));
#15936=CARTESIAN_POINT('Ctrl Pts',(-0.796034321106412,21.8063297959755,
0.));
#15937=CARTESIAN_POINT('Ctrl Pts',(-0.766119391688713,21.8612367655148,
0.));
#15938=CARTESIAN_POINT('Ctrl Pts',(-0.740879090965097,21.9069273598709,
0.));
#15939=CARTESIAN_POINT('Ctrl Pts',(-0.720488353007147,21.9434380560096,
0.));
#15940=CARTESIAN_POINT('Ctrl Pts',(-0.70508375626176,21.970797600548,0.));
#15941=CARTESIAN_POINT('Ctrl Pts',(-0.69476445021958,21.9890268624765,0.));
#15942=CARTESIAN_POINT('',(-0.694764450219644,21.9890268624765,13.));
#15943=CARTESIAN_POINT('Ctrl Pts',(-0.69476445021958,21.9890268624765,13.));
#15944=CARTESIAN_POINT('Ctrl Pts',(-0.745561803283239,21.8992923152799,
13.));
#15945=CARTESIAN_POINT('Ctrl Pts',(-0.794921865564174,21.8092529630784,
13.));
#15946=CARTESIAN_POINT('Ctrl Pts',(-0.842819260919079,21.7189137537155,
13.));
#15947=CARTESIAN_POINT('Ctrl Pts',(-0.922187323998701,21.5692177626466,
13.));
#15948=CARTESIAN_POINT('Ctrl Pts',(-0.997528955439908,21.4187072727147,
13.));
#15949=CARTESIAN_POINT('Ctrl Pts',(-1.06858105391185,21.2675022584072,13.));
#15950=CARTESIAN_POINT('Ctrl Pts',(-1.12319586329668,21.1512772177393,13.));
#15951=CARTESIAN_POINT('Ctrl Pts',(-1.17527598661216,21.0346391558834,13.));
#15952=CARTESIAN_POINT('Ctrl Pts',(-1.22467603855632,20.917644242923,13.));
#15953=CARTESIAN_POINT('Ctrl Pts',(-1.27785400417095,20.7917020381349,13.));
#15954=CARTESIAN_POINT('Ctrl Pts',(-1.32793259662342,20.6653453744634,13.));
#15955=CARTESIAN_POINT('Ctrl Pts',(-1.37465955681607,20.5386490834201,13.));
#15956=CARTESIAN_POINT('Ctrl Pts',(-1.40052887118435,20.4685065753523,13.));
#15957=CARTESIAN_POINT('Ctrl Pts',(-1.42537603688911,20.3982600582948,13.));
#15958=CARTESIAN_POINT('Ctrl Pts',(-1.44915458805604,20.3279233189672,13.));
#15959=CARTESIAN_POINT('Ctrl Pts',(-1.47206853306895,20.2601440768247,13.));
#15960=CARTESIAN_POINT('Ctrl Pts',(-1.49398338579287,20.1922811204633,13.));
#15961=CARTESIAN_POINT('Ctrl Pts',(-1.51482335730943,20.1243481779698,13.));
#15962=CARTESIAN_POINT('Ctrl Pts',(-1.53283548365772,20.0656332827775,13.));
#15963=CARTESIAN_POINT('Ctrl Pts',(-1.55004791448615,20.0068660712896,13.));
#15964=CARTESIAN_POINT('Ctrl Pts',(-1.5664583915576,19.9480555831788,13.));
#15965=CARTESIAN_POINT('Ctrl Pts',(-1.57823544845321,19.9058499567655,13.));
#15966=CARTESIAN_POINT('Ctrl Pts',(-1.58960230238178,19.8636220200104,13.));
#15967=CARTESIAN_POINT('Ctrl Pts',(-1.60051957231072,19.8213758740547,13.));
#15968=CARTESIAN_POINT('Ctrl Pts',(-1.61125906811029,19.7798176539142,13.));
#15969=CARTESIAN_POINT('Ctrl Pts',(-1.62155711739663,19.7382418845082,13.));
#15970=CARTESIAN_POINT('Ctrl Pts',(-1.631361434785,19.6966529617546,13.));
#15971=CARTESIAN_POINT('Ctrl Pts',(-1.63986235395436,19.6605929224204,13.));
#15972=CARTESIAN_POINT('Ctrl Pts',(-1.64798961246616,19.6245230263946,13.));
#15973=CARTESIAN_POINT('Ctrl Pts',(-1.6557586144792,19.5884457882424,13.));
#15974=CARTESIAN_POINT('Ctrl Pts',(-1.66279554781242,19.5557680879024,13.));
#15975=CARTESIAN_POINT('Ctrl Pts',(-1.66954412482931,19.5230842952898,13.));
#15976=CARTESIAN_POINT('Ctrl Pts',(-1.67602787922142,19.4903963526387,13.));
#15977=CARTESIAN_POINT('Ctrl Pts',(-1.68148945143256,19.4628617564117,13.));
#15978=CARTESIAN_POINT('Ctrl Pts',(-1.68676485592428,19.435324196667,13.));
#15979=CARTESIAN_POINT('Ctrl Pts',(-1.69183425662716,19.4077853967291,13.));
#15980=CARTESIAN_POINT('Ctrl Pts',(-1.69917023102265,19.3679337568473,13.));
#15981=CARTESIAN_POINT('Ctrl Pts',(-1.70607400305428,19.3280794804219,13.));
#15982=CARTESIAN_POINT('Ctrl Pts',(-1.71232694126836,19.2882303925697,13.));
#15983=CARTESIAN_POINT('Ctrl Pts',(-1.71610520911737,19.2641520277611,13.));
#15984=CARTESIAN_POINT('Ctrl Pts',(-1.71964237037416,19.2400756157958,13.));
#15985=CARTESIAN_POINT('Ctrl Pts',(-1.72291205968776,19.2160028183594,13.));
#15986=CARTESIAN_POINT('Ctrl Pts',(-1.7259276330568,19.193800927016,13.));
#15987=CARTESIAN_POINT('Ctrl Pts',(-1.72871436969152,19.171602126741,13.));
#15988=CARTESIAN_POINT('Ctrl Pts',(-1.73129733453724,19.1494073128219,13.));
#15989=CARTESIAN_POINT('Ctrl Pts',(-1.73485046444234,19.1188760970354,13.));
#15990=CARTESIAN_POINT('Ctrl Pts',(-1.73802530995816,19.0883522198594,13.));
#15991=CARTESIAN_POINT('Ctrl Pts',(-1.7409726387683,19.0578380260009,13.));
#15992=CARTESIAN_POINT('Ctrl Pts',(-1.74284247674286,19.0384792770743,13.));
#15993=CARTESIAN_POINT('Ctrl Pts',(-1.74462241724203,19.0191244315393,13.));
#15994=CARTESIAN_POINT('Ctrl Pts',(-1.74632097576209,18.9997750006553,13.));
#15995=CARTESIAN_POINT('Ctrl Pts',(-1.74784535297286,18.9824097870743,13.));
#15996=CARTESIAN_POINT('Ctrl Pts',(-1.74930491161852,18.9650489252156,13.));
#15997=CARTESIAN_POINT('Ctrl Pts',(-1.75066513119703,18.9476944343612,13.));
#15998=CARTESIAN_POINT('Ctrl Pts',(-1.75209499287824,18.9294514081162,13.));
#15999=CARTESIAN_POINT('Ctrl Pts',(-1.75341524153751,18.9112154258559,13.));
#16000=CARTESIAN_POINT('Ctrl Pts',(-1.7545234786503,18.8929901414275,13.));
#16001=CARTESIAN_POINT('Ctrl Pts',(-1.7563642580427,18.8627179843144,13.));
#16002=CARTESIAN_POINT('Ctrl Pts',(-1.75761169393889,18.8324756678297,13.));
#16003=CARTESIAN_POINT('Ctrl Pts',(-1.75764008468139,18.8022820950122,13.));
#16004=CARTESIAN_POINT('Ctrl Pts',(-1.75765574034722,18.7856322843864,13.));
#16005=CARTESIAN_POINT('Ctrl Pts',(-1.75729933637085,18.7689972916942,13.));
#16006=CARTESIAN_POINT('Ctrl Pts',(-1.75649392367898,18.752379304385,13.));
#16007=CARTESIAN_POINT('Ctrl Pts',(-1.75583876199516,18.7388614288199,13.));
#16008=CARTESIAN_POINT('Ctrl Pts',(-1.75488656240175,18.7253548001799,13.));
#16009=CARTESIAN_POINT('Ctrl Pts',(-1.75362185428836,18.7118598491961,13.));
#16010=CARTESIAN_POINT('',(-0.694764450219644,21.9890268624765,0.));
#16011=CARTESIAN_POINT('Origin',(0.,5.6665783176868E-12,0.));
#16012=CARTESIAN_POINT('',(0.694764450219583,21.9890268624765,0.));
#16013=CARTESIAN_POINT('Origin',(0.,5.6665783176868E-12,0.));
#16014=CARTESIAN_POINT('',(0.694764450219583,21.9890268624765,13.));
#16015=CARTESIAN_POINT('Origin',(0.,5.6665783176868E-12,13.));
#16016=CARTESIAN_POINT('',(0.694764450219583,21.9890268624765,0.));
#16017=CARTESIAN_POINT('Ctrl Pts',(1.75362185428837,18.7118598491961,0.));
#16018=CARTESIAN_POINT('Ctrl Pts',(1.75362185428837,18.7118598491961,21.));
#16019=CARTESIAN_POINT('Ctrl Pts',(1.75450132833464,18.7212441956871,0.));
#16020=CARTESIAN_POINT('Ctrl Pts',(1.75450132833464,18.7212441956871,21.));
#16021=CARTESIAN_POINT('Ctrl Pts',(1.75601041697575,18.7400222442427,0.));
#16022=CARTESIAN_POINT('Ctrl Pts',(1.75601041697575,18.7400222442427,21.));
#16023=CARTESIAN_POINT('Ctrl Pts',(1.75752447968136,18.7682173836138,0.));
#16024=CARTESIAN_POINT('Ctrl Pts',(1.75752447968136,18.7682173836138,21.));
#16025=CARTESIAN_POINT('Ctrl Pts',(1.7581175236483,18.8058650094753,0.));
#16026=CARTESIAN_POINT('Ctrl Pts',(1.7581175236483,18.8058650094753,21.));
#16027=CARTESIAN_POINT('Ctrl Pts',(1.75690876962597,18.8530026395886,0.));
#16028=CARTESIAN_POINT('Ctrl Pts',(1.75690876962597,18.8530026395886,21.));
#16029=CARTESIAN_POINT('Ctrl Pts',(1.75429229572775,18.9002024267872,0.));
#16030=CARTESIAN_POINT('Ctrl Pts',(1.75429229572775,18.9002024267872,21.));
#16031=CARTESIAN_POINT('Ctrl Pts',(1.75080409924533,18.947447637865,0.));
#16032=CARTESIAN_POINT('Ctrl Pts',(1.75080409924533,18.947447637865,21.));
#16033=CARTESIAN_POINT('Ctrl Pts',(1.74684309825012,18.9947239970259,0.));
#16034=CARTESIAN_POINT('Ctrl Pts',(1.74684309825012,18.9947239970259,21.));
#16035=CARTESIAN_POINT('Ctrl Pts',(1.74256297552949,19.0420224296189,0.));
#16036=CARTESIAN_POINT('Ctrl Pts',(1.74256297552949,19.0420224296189,21.));
#16037=CARTESIAN_POINT('Ctrl Pts',(1.73795301169841,19.0893375576541,0.));
#16038=CARTESIAN_POINT('Ctrl Pts',(1.73795301169841,19.0893375576541,21.));
#16039=CARTESIAN_POINT('Ctrl Pts',(1.73290313712353,19.1366665585833,0.));
#16040=CARTESIAN_POINT('Ctrl Pts',(1.73290313712353,19.1366665585833,21.));
#16041=CARTESIAN_POINT('Ctrl Pts',(1.72727220327098,19.1840079312107,0.));
#16042=CARTESIAN_POINT('Ctrl Pts',(1.72727220327098,19.1840079312107,21.));
#16043=CARTESIAN_POINT('Ctrl Pts',(1.72096104670234,19.2313602042899,0.));
#16044=CARTESIAN_POINT('Ctrl Pts',(1.72096104670234,19.2313602042899,21.));
#16045=CARTESIAN_POINT('Ctrl Pts',(1.71396454346262,19.2787209722437,0.));
#16046=CARTESIAN_POINT('Ctrl Pts',(1.71396454346262,19.2787209722437,21.));
#16047=CARTESIAN_POINT('Ctrl Pts',(1.70633457265124,19.3260873558094,0.));
#16048=CARTESIAN_POINT('Ctrl Pts',(1.70633457265124,19.3260873558094,21.));
#16049=CARTESIAN_POINT('Ctrl Pts',(1.69815571801252,19.3734562555057,0.));
#16050=CARTESIAN_POINT('Ctrl Pts',(1.69815571801252,19.3734562555057,21.));
#16051=CARTESIAN_POINT('Ctrl Pts',(1.68951753233571,19.4208246682917,0.));
#16052=CARTESIAN_POINT('Ctrl Pts',(1.68951753233571,19.4208246682917,21.));
#16053=CARTESIAN_POINT('Ctrl Pts',(1.68048476382294,19.4681900187091,0.));
#16054=CARTESIAN_POINT('Ctrl Pts',(1.68048476382294,19.4681900187091,21.));
#16055=CARTESIAN_POINT('Ctrl Pts',(1.67107974760949,19.5155503513712,0.));
#16056=CARTESIAN_POINT('Ctrl Pts',(1.67107974760949,19.5155503513712,21.));
#16057=CARTESIAN_POINT('Ctrl Pts',(1.66129908621006,19.5629041190868,0.));
#16058=CARTESIAN_POINT('Ctrl Pts',(1.66129908621006,19.5629041190868,21.));
#16059=CARTESIAN_POINT('Ctrl Pts',(1.65112409599283,19.6102500448855,0.));
#16060=CARTESIAN_POINT('Ctrl Pts',(1.65112409599283,19.6102500448855,21.));
#16061=CARTESIAN_POINT('Ctrl Pts',(1.64053294677821,19.6575869645839,0.));
#16062=CARTESIAN_POINT('Ctrl Pts',(1.64053294677821,19.6575869645839,21.));
#16063=CARTESIAN_POINT('Ctrl Pts',(1.62951389038422,19.7049136553525,0.));
#16064=CARTESIAN_POINT('Ctrl Pts',(1.62951389038422,19.7049136553525,21.));
#16065=CARTESIAN_POINT('Ctrl Pts',(1.61807191996834,19.7522287462982,0.));
#16066=CARTESIAN_POINT('Ctrl Pts',(1.61807191996834,19.7522287462982,21.));
#16067=CARTESIAN_POINT('Ctrl Pts',(1.60622162219699,19.7995308006834,0.));
#16068=CARTESIAN_POINT('Ctrl Pts',(1.60622162219699,19.7995308006834,21.));
#16069=CARTESIAN_POINT('Ctrl Pts',(1.59398289700559,19.8468183626037,0.));
#16070=CARTESIAN_POINT('Ctrl Pts',(1.59398289700559,19.8468183626037,21.));
#16071=CARTESIAN_POINT('Ctrl Pts',(1.58137589158952,19.8940900137801,0.));
#16072=CARTESIAN_POINT('Ctrl Pts',(1.58137589158952,19.8940900137801,21.));
#16073=CARTESIAN_POINT('Ctrl Pts',(1.56841542790452,19.9413444362352,0.));
#16074=CARTESIAN_POINT('Ctrl Pts',(1.56841542790452,19.9413444362352,21.));
#16075=CARTESIAN_POINT('Ctrl Pts',(1.55510860515914,19.9885804375097,0.));
#16076=CARTESIAN_POINT('Ctrl Pts',(1.55510860515914,19.9885804375097,21.));
#16077=CARTESIAN_POINT('Ctrl Pts',(1.54145790302918,20.0357969106526,0.));
#16078=CARTESIAN_POINT('Ctrl Pts',(1.54145790302918,20.0357969106526,21.));
#16079=CARTESIAN_POINT('Ctrl Pts',(1.52746305716964,20.0829928089241,0.));
#16080=CARTESIAN_POINT('Ctrl Pts',(1.52746305716964,20.0829928089241,21.));
#16081=CARTESIAN_POINT('Ctrl Pts',(1.51312326913583,20.1301671167606,0.));
#16082=CARTESIAN_POINT('Ctrl Pts',(1.51312326913583,20.1301671167606,21.));
#16083=CARTESIAN_POINT('Ctrl Pts',(1.49843965844502,20.1773188177942,0.));
#16084=CARTESIAN_POINT('Ctrl Pts',(1.49843965844502,20.1773188177942,21.));
#16085=CARTESIAN_POINT('Ctrl Pts',(1.48341623961914,20.224446881308,0.));
#16086=CARTESIAN_POINT('Ctrl Pts',(1.48341623961914,20.224446881308,21.));
#16087=CARTESIAN_POINT('Ctrl Pts',(1.46805861808021,20.2715502770004,0.));
#16088=CARTESIAN_POINT('Ctrl Pts',(1.46805861808021,20.2715502770004,21.));
#16089=CARTESIAN_POINT('Ctrl Pts',(1.45237321894404,20.3186279833818,0.));
#16090=CARTESIAN_POINT('Ctrl Pts',(1.45237321894404,20.3186279833818,21.));
#16091=CARTESIAN_POINT('Ctrl Pts',(1.43636637152782,20.3656789980171,0.));
#16092=CARTESIAN_POINT('Ctrl Pts',(1.43636637152782,20.3656789980171,21.));
#16093=CARTESIAN_POINT('Ctrl Pts',(1.4200432946371,20.4127023494155,0.));
#16094=CARTESIAN_POINT('Ctrl Pts',(1.4200432946371,20.4127023494155,21.));
#16095=CARTESIAN_POINT('Ctrl Pts',(1.40340771617025,20.4596971004275,0.));
#16096=CARTESIAN_POINT('Ctrl Pts',(1.40340771617025,20.4596971004275,21.));
#16097=CARTESIAN_POINT('Ctrl Pts',(1.38646244026049,20.5066623390132,0.));
#16098=CARTESIAN_POINT('Ctrl Pts',(1.38646244026049,20.5066623390132,21.));
#16099=CARTESIAN_POINT('Ctrl Pts',(1.36920969340018,20.5535971721246,0.));
#16100=CARTESIAN_POINT('Ctrl Pts',(1.36920969340018,20.5535971721246,21.));
#16101=CARTESIAN_POINT('Ctrl Pts',(1.35165153211253,20.6005007190809,0.));
#16102=CARTESIAN_POINT('Ctrl Pts',(1.35165153211253,20.6005007190809,21.));
#16103=CARTESIAN_POINT('Ctrl Pts',(1.3337902972259,20.6473721041685,0.));
#16104=CARTESIAN_POINT('Ctrl Pts',(1.3337902972259,20.6473721041685,21.));
#16105=CARTESIAN_POINT('Ctrl Pts',(1.31562879653596,20.694210454218,0.));
#16106=CARTESIAN_POINT('Ctrl Pts',(1.31562879653596,20.694210454218,21.));
#16107=CARTESIAN_POINT('Ctrl Pts',(1.2971700649115,20.7410149035348,0.));
#16108=CARTESIAN_POINT('Ctrl Pts',(1.2971700649115,20.7410149035348,21.));
#16109=CARTESIAN_POINT('Ctrl Pts',(1.27841722479262,20.7877845975367,0.));
#16110=CARTESIAN_POINT('Ctrl Pts',(1.27841722479262,20.7877845975367,21.));
#16111=CARTESIAN_POINT('Ctrl Pts',(1.25937332001005,20.83451869657,0.));
#16112=CARTESIAN_POINT('Ctrl Pts',(1.25937332001005,20.83451869657,21.));
#16113=CARTESIAN_POINT('Ctrl Pts',(1.24004113517905,20.881216381382,0.));
#16114=CARTESIAN_POINT('Ctrl Pts',(1.24004113517905,20.881216381382,21.));
#16115=CARTESIAN_POINT('Ctrl Pts',(1.22042312071096,20.9278768531175,0.));
#16116=CARTESIAN_POINT('Ctrl Pts',(1.22042312071096,20.9278768531175,21.));
#16117=CARTESIAN_POINT('Ctrl Pts',(1.20052150219503,20.9744993243732,0.));
#16118=CARTESIAN_POINT('Ctrl Pts',(1.20052150219503,20.9744993243732,21.));
#16119=CARTESIAN_POINT('Ctrl Pts',(1.18033835060894,21.0210830121673,0.));
#16120=CARTESIAN_POINT('Ctrl Pts',(1.18033835060894,21.0210830121673,21.));
#16121=CARTESIAN_POINT('Ctrl Pts',(1.15987566445807,21.0676271313238,0.));
#16122=CARTESIAN_POINT('Ctrl Pts',(1.15987566445807,21.0676271313238,21.));
#16123=CARTESIAN_POINT('Ctrl Pts',(1.13913546246555,21.1141308858087,0.));
#16124=CARTESIAN_POINT('Ctrl Pts',(1.13913546246555,21.1141308858087,21.));
#16125=CARTESIAN_POINT('Ctrl Pts',(1.11811982787747,21.1605934684164,0.));
#16126=CARTESIAN_POINT('Ctrl Pts',(1.11811982787747,21.1605934684164,21.));
#16127=CARTESIAN_POINT('Ctrl Pts',(1.09683084929266,21.2070140764156,0.));
#16128=CARTESIAN_POINT('Ctrl Pts',(1.09683084929266,21.2070140764156,21.));
#16129=CARTESIAN_POINT('Ctrl Pts',(1.07527058431887,21.2533919248553,0.));
#16130=CARTESIAN_POINT('Ctrl Pts',(1.07527058431887,21.2533919248553,21.));
#16131=CARTESIAN_POINT('Ctrl Pts',(1.05344101900192,21.2997262593683,0.));
#16132=CARTESIAN_POINT('Ctrl Pts',(1.05344101900192,21.2997262593683,21.));
#16133=CARTESIAN_POINT('Ctrl Pts',(1.03134402396953,21.3460163737343,0.));
#16134=CARTESIAN_POINT('Ctrl Pts',(1.03134402396953,21.3460163737343,21.));
#16135=CARTESIAN_POINT('Ctrl Pts',(1.00898133629988,21.3922616124166,0.));
#16136=CARTESIAN_POINT('Ctrl Pts',(1.00898133629988,21.3922616124166,21.));
#16137=CARTESIAN_POINT('Ctrl Pts',(0.986354611081136,21.4384613333266,0.));
#16138=CARTESIAN_POINT('Ctrl Pts',(0.986354611081136,21.4384613333266,21.));
#16139=CARTESIAN_POINT('Ctrl Pts',(0.963465462815772,21.4846148770804,0.));
#16140=CARTESIAN_POINT('Ctrl Pts',(0.963465462815772,21.4846148770804,21.));
#16141=CARTESIAN_POINT('Ctrl Pts',(0.940315509525153,21.5307215366685,0.));
#16142=CARTESIAN_POINT('Ctrl Pts',(0.940315509525153,21.5307215366685,21.));
#16143=CARTESIAN_POINT('Ctrl Pts',(0.916906425150855,21.5767805209408,0.));
#16144=CARTESIAN_POINT('Ctrl Pts',(0.916906425150855,21.5767805209408,21.));
#16145=CARTESIAN_POINT('Ctrl Pts',(0.893239967513676,21.6227909401433,0.));
#16146=CARTESIAN_POINT('Ctrl Pts',(0.893239967513676,21.6227909401433,21.));
#16147=CARTESIAN_POINT('Ctrl Pts',(0.8693178977141,21.6687518829182,0.));
#16148=CARTESIAN_POINT('Ctrl Pts',(0.8693178977141,21.6687518829182,21.));
#16149=CARTESIAN_POINT('Ctrl Pts',(0.845141916726561,21.7146624809285,0.));
#16150=CARTESIAN_POINT('Ctrl Pts',(0.845141916726561,21.7146624809285,21.));
#16151=CARTESIAN_POINT('Ctrl Pts',(0.820713597934078,21.7605219769118,0.));
#16152=CARTESIAN_POINT('Ctrl Pts',(0.820713597934078,21.7605219769118,21.));
#16153=CARTESIAN_POINT('Ctrl Pts',(0.796034321106414,21.8063297959755,0.));
#16154=CARTESIAN_POINT('Ctrl Pts',(0.796034321106414,21.8063297959755,21.));
#16155=CARTESIAN_POINT('Ctrl Pts',(0.771105213258333,21.8520856039249,0.));
#16156=CARTESIAN_POINT('Ctrl Pts',(0.771105213258333,21.8520856039249,21.));
#16157=CARTESIAN_POINT('Ctrl Pts',(0.745927151109822,21.8977892409997,0.));
#16158=CARTESIAN_POINT('Ctrl Pts',(0.745927151109822,21.8977892409997,21.));
#16159=CARTESIAN_POINT('Ctrl Pts',(0.725586037496637,21.9343103819749,0.));
#16160=CARTESIAN_POINT('Ctrl Pts',(0.725586037496637,21.9343103819749,21.));
#16161=CARTESIAN_POINT('Ctrl Pts',(0.710218621843558,21.9616777523685,0.));
#16162=CARTESIAN_POINT('Ctrl Pts',(0.710218621843558,21.9616777523685,21.));
#16163=CARTESIAN_POINT('Ctrl Pts',(0.699924103234224,21.9799122315157,0.));
#16164=CARTESIAN_POINT('Ctrl Pts',(0.699924103234224,21.9799122315157,21.));
#16165=CARTESIAN_POINT('Ctrl Pts',(0.694764450219582,21.9890268624765,0.));
#16166=CARTESIAN_POINT('Ctrl Pts',(0.694764450219582,21.9890268624765,21.));
#16167=CARTESIAN_POINT('Ctrl Pts',(1.75362185428837,18.7118598491961,0.));
#16168=CARTESIAN_POINT('Ctrl Pts',(1.75450132833464,18.7212441956871,0.));
#16169=CARTESIAN_POINT('Ctrl Pts',(1.75601041697575,18.7400222442427,0.));
#16170=CARTESIAN_POINT('Ctrl Pts',(1.75752447968136,18.7682173836138,0.));
#16171=CARTESIAN_POINT('Ctrl Pts',(1.7581175236483,18.8058650094753,0.));
#16172=CARTESIAN_POINT('Ctrl Pts',(1.75690876962597,18.8530026395886,0.));
#16173=CARTESIAN_POINT('Ctrl Pts',(1.75429229572775,18.9002024267872,0.));
#16174=CARTESIAN_POINT('Ctrl Pts',(1.75080409924533,18.947447637865,0.));
#16175=CARTESIAN_POINT('Ctrl Pts',(1.74684309825012,18.9947239970259,0.));
#16176=CARTESIAN_POINT('Ctrl Pts',(1.74256297552949,19.0420224296189,0.));
#16177=CARTESIAN_POINT('Ctrl Pts',(1.73795301169841,19.0893375576541,0.));
#16178=CARTESIAN_POINT('Ctrl Pts',(1.73290313712353,19.1366665585833,0.));
#16179=CARTESIAN_POINT('Ctrl Pts',(1.72727220327098,19.1840079312107,0.));
#16180=CARTESIAN_POINT('Ctrl Pts',(1.72096104670234,19.2313602042899,0.));
#16181=CARTESIAN_POINT('Ctrl Pts',(1.71396454346262,19.2787209722437,0.));
#16182=CARTESIAN_POINT('Ctrl Pts',(1.70633457265124,19.3260873558094,0.));
#16183=CARTESIAN_POINT('Ctrl Pts',(1.69815571801252,19.3734562555057,0.));
#16184=CARTESIAN_POINT('Ctrl Pts',(1.68951753233571,19.4208246682917,0.));
#16185=CARTESIAN_POINT('Ctrl Pts',(1.68048476382294,19.4681900187091,0.));
#16186=CARTESIAN_POINT('Ctrl Pts',(1.67107974760949,19.5155503513712,0.));
#16187=CARTESIAN_POINT('Ctrl Pts',(1.66129908621006,19.5629041190868,0.));
#16188=CARTESIAN_POINT('Ctrl Pts',(1.65112409599283,19.6102500448855,0.));
#16189=CARTESIAN_POINT('Ctrl Pts',(1.64053294677821,19.6575869645839,0.));
#16190=CARTESIAN_POINT('Ctrl Pts',(1.62951389038422,19.7049136553525,0.));
#16191=CARTESIAN_POINT('Ctrl Pts',(1.61807191996834,19.7522287462982,0.));
#16192=CARTESIAN_POINT('Ctrl Pts',(1.60622162219699,19.7995308006834,0.));
#16193=CARTESIAN_POINT('Ctrl Pts',(1.59398289700559,19.8468183626037,0.));
#16194=CARTESIAN_POINT('Ctrl Pts',(1.58137589158952,19.8940900137801,0.));
#16195=CARTESIAN_POINT('Ctrl Pts',(1.56841542790452,19.9413444362352,0.));
#16196=CARTESIAN_POINT('Ctrl Pts',(1.55510860515914,19.9885804375097,0.));
#16197=CARTESIAN_POINT('Ctrl Pts',(1.54145790302918,20.0357969106526,0.));
#16198=CARTESIAN_POINT('Ctrl Pts',(1.52746305716964,20.0829928089241,0.));
#16199=CARTESIAN_POINT('Ctrl Pts',(1.51312326913583,20.1301671167606,0.));
#16200=CARTESIAN_POINT('Ctrl Pts',(1.49843965844502,20.1773188177942,0.));
#16201=CARTESIAN_POINT('Ctrl Pts',(1.48341623961914,20.224446881308,0.));
#16202=CARTESIAN_POINT('Ctrl Pts',(1.46805861808021,20.2715502770004,0.));
#16203=CARTESIAN_POINT('Ctrl Pts',(1.45237321894404,20.3186279833818,0.));
#16204=CARTESIAN_POINT('Ctrl Pts',(1.43636637152782,20.3656789980171,0.));
#16205=CARTESIAN_POINT('Ctrl Pts',(1.4200432946371,20.4127023494155,0.));
#16206=CARTESIAN_POINT('Ctrl Pts',(1.40340771617025,20.4596971004275,0.));
#16207=CARTESIAN_POINT('Ctrl Pts',(1.38646244026049,20.5066623390132,0.));
#16208=CARTESIAN_POINT('Ctrl Pts',(1.36920969340018,20.5535971721246,0.));
#16209=CARTESIAN_POINT('Ctrl Pts',(1.35165153211253,20.6005007190809,0.));
#16210=CARTESIAN_POINT('Ctrl Pts',(1.3337902972259,20.6473721041685,0.));
#16211=CARTESIAN_POINT('Ctrl Pts',(1.31562879653596,20.694210454218,0.));
#16212=CARTESIAN_POINT('Ctrl Pts',(1.2971700649115,20.7410149035348,0.));
#16213=CARTESIAN_POINT('Ctrl Pts',(1.27841722479262,20.7877845975367,0.));
#16214=CARTESIAN_POINT('Ctrl Pts',(1.25937332001005,20.83451869657,0.));
#16215=CARTESIAN_POINT('Ctrl Pts',(1.24004113517905,20.881216381382,0.));
#16216=CARTESIAN_POINT('Ctrl Pts',(1.22042312071096,20.9278768531175,0.));
#16217=CARTESIAN_POINT('Ctrl Pts',(1.20052150219503,20.9744993243732,0.));
#16218=CARTESIAN_POINT('Ctrl Pts',(1.18033835060894,21.0210830121673,0.));
#16219=CARTESIAN_POINT('Ctrl Pts',(1.15987566445807,21.0676271313238,0.));
#16220=CARTESIAN_POINT('Ctrl Pts',(1.13913546246555,21.1141308858087,0.));
#16221=CARTESIAN_POINT('Ctrl Pts',(1.11811982787747,21.1605934684164,0.));
#16222=CARTESIAN_POINT('Ctrl Pts',(1.09683084929266,21.2070140764156,0.));
#16223=CARTESIAN_POINT('Ctrl Pts',(1.07527058431887,21.2533919248553,0.));
#16224=CARTESIAN_POINT('Ctrl Pts',(1.05344101900192,21.2997262593683,0.));
#16225=CARTESIAN_POINT('Ctrl Pts',(1.03134402396953,21.3460163737343,0.));
#16226=CARTESIAN_POINT('Ctrl Pts',(1.00898133629988,21.3922616124166,0.));
#16227=CARTESIAN_POINT('Ctrl Pts',(0.986354611081136,21.4384613333266,0.));
#16228=CARTESIAN_POINT('Ctrl Pts',(0.963465462815772,21.4846148770804,0.));
#16229=CARTESIAN_POINT('Ctrl Pts',(0.940315509525153,21.5307215366685,0.));
#16230=CARTESIAN_POINT('Ctrl Pts',(0.916906425150855,21.5767805209408,0.));
#16231=CARTESIAN_POINT('Ctrl Pts',(0.893239967513676,21.6227909401433,0.));
#16232=CARTESIAN_POINT('Ctrl Pts',(0.8693178977141,21.6687518829182,0.));
#16233=CARTESIAN_POINT('Ctrl Pts',(0.845141916726561,21.7146624809285,0.));
#16234=CARTESIAN_POINT('Ctrl Pts',(0.820713597934078,21.7605219769118,0.));
#16235=CARTESIAN_POINT('Ctrl Pts',(0.796034321106414,21.8063297959755,0.));
#16236=CARTESIAN_POINT('Ctrl Pts',(0.766119391688716,21.8612367655148,0.));
#16237=CARTESIAN_POINT('Ctrl Pts',(0.740879090965098,21.9069273598709,0.));
#16238=CARTESIAN_POINT('Ctrl Pts',(0.72048835300715,21.9434380560096,0.));
#16239=CARTESIAN_POINT('Ctrl Pts',(0.705083756261762,21.970797600548,0.));
#16240=CARTESIAN_POINT('Ctrl Pts',(0.694764450219582,21.9890268624765,0.));
#16241=CARTESIAN_POINT('Ctrl Pts',(1.75362185428837,18.7118598491961,13.));
#16242=CARTESIAN_POINT('Ctrl Pts',(1.75510417082368,18.7276767707252,13.));
#16243=CARTESIAN_POINT('Ctrl Pts',(1.75615601189427,18.7435097672895,13.));
#16244=CARTESIAN_POINT('Ctrl Pts',(1.75680608702498,18.7593580381841,13.));
#16245=CARTESIAN_POINT('Ctrl Pts',(1.75756802370039,18.7779333970402,13.));
#16246=CARTESIAN_POINT('Ctrl Pts',(1.75777887919059,18.7965297250687,13.));
#16247=CARTESIAN_POINT('Ctrl Pts',(1.75755628860693,18.8151436576359,13.));
#16248=CARTESIAN_POINT('Ctrl Pts',(1.75724309300303,18.8413343515796,13.));
#16249=CARTESIAN_POINT('Ctrl Pts',(1.756078938996,18.8675597701072,13.));
#16250=CARTESIAN_POINT('Ctrl Pts',(1.75447363677689,18.8938074357123,13.));
#16251=CARTESIAN_POINT('Ctrl Pts',(1.7534058576267,18.9112662728963,13.));
#16252=CARTESIAN_POINT('Ctrl Pts',(1.75214492935998,18.9287348768824,13.));
#16253=CARTESIAN_POINT('Ctrl Pts',(1.75078122387634,18.946210028328,13.));
#16254=CARTESIAN_POINT('Ctrl Pts',(1.74934570031147,18.9646054898119,13.));
#16255=CARTESIAN_POINT('Ctrl Pts',(1.74779717198878,18.983008180503,13.));
#16256=CARTESIAN_POINT('Ctrl Pts',(1.74617674699319,19.0014156957761,13.));
#16257=CARTESIAN_POINT('Ctrl Pts',(1.7443771763328,19.0218582491225,13.));
#16258=CARTESIAN_POINT('Ctrl Pts',(1.74248762596105,19.0423067706001,13.));
#16259=CARTESIAN_POINT('Ctrl Pts',(1.74049525500457,19.0627595477229,13.));
#16260=CARTESIAN_POINT('Ctrl Pts',(1.73749165908592,19.0935931019321,13.));
#16261=CARTESIAN_POINT('Ctrl Pts',(1.73424805120572,19.1244363539441,13.));
#16262=CARTESIAN_POINT('Ctrl Pts',(1.73060838684995,19.1552870037662,13.));
#16263=CARTESIAN_POINT('Ctrl Pts',(1.72796425026689,19.177699326396,13.));
#16264=CARTESIAN_POINT('Ctrl Pts',(1.72510779282552,19.2001156537969,13.));
#16265=CARTESIAN_POINT('Ctrl Pts',(1.72201836571307,19.2225350169791,13.));
#16266=CARTESIAN_POINT('Ctrl Pts',(1.7182418056105,19.2499407687372,13.));
#16267=CARTESIAN_POINT('Ctrl Pts',(1.71411839343916,19.2773510352421,13.));
#16268=CARTESIAN_POINT('Ctrl Pts',(1.70969587297501,19.3047632983536,13.));
#16269=CARTESIAN_POINT('Ctrl Pts',(1.7049188168855,19.3343730920189,13.));
#16270=CARTESIAN_POINT('Ctrl Pts',(1.69979875336796,19.3639851445093,13.));
#16271=CARTESIAN_POINT('Ctrl Pts',(1.69442732753607,19.3935962281232,13.));
#16272=CARTESIAN_POINT('Ctrl Pts',(1.68946845243963,19.4209330414214,13.));
#16273=CARTESIAN_POINT('Ctrl Pts',(1.68429785630468,19.4482690053315,13.));
#16274=CARTESIAN_POINT('Ctrl Pts',(1.67894398812285,19.4756022976083,13.));
#16275=CARTESIAN_POINT('Ctrl Pts',(1.6716704833028,19.5127359785976,13.));
#16276=CARTESIAN_POINT('Ctrl Pts',(1.66405675112745,19.5498647401943,13.));
#16277=CARTESIAN_POINT('Ctrl Pts',(1.65607285223626,19.5869856493607,13.));
#16278=CARTESIAN_POINT('Ctrl Pts',(1.64836856224328,19.6228065249654,13.));
#16279=CARTESIAN_POINT('Ctrl Pts',(1.64031177033463,19.658620192316,13.));
#16280=CARTESIAN_POINT('Ctrl Pts',(1.6318863792002,19.6944241980793,13.));
#16281=CARTESIAN_POINT('Ctrl Pts',(1.62044024926504,19.743064943135,13.));
#16282=CARTESIAN_POINT('Ctrl Pts',(1.60831707819419,19.7916877990049,13.));
#16283=CARTESIAN_POINT('Ctrl Pts',(1.59560243915133,19.8402857465542,13.));
#16284=CARTESIAN_POINT('Ctrl Pts',(1.58442654784796,19.8830022859342,13.));
#16285=CARTESIAN_POINT('Ctrl Pts',(1.57280052808028,19.9256995149414,13.));
#16286=CARTESIAN_POINT('Ctrl Pts',(1.56075644053507,19.9683733416781,13.));
#16287=CARTESIAN_POINT('Ctrl Pts',(1.5430005314399,20.0312849226041,13.));
#16288=CARTESIAN_POINT('Ctrl Pts',(1.52432694535417,20.0941457149226,13.));
#16289=CARTESIAN_POINT('Ctrl Pts',(1.50474000386434,20.1569447709389,13.));
#16290=CARTESIAN_POINT('Ctrl Pts',(1.48002109253598,20.2361977925492,13.));
#16291=CARTESIAN_POINT('Ctrl Pts',(1.45385270864268,20.3153523889509,13.));
#16292=CARTESIAN_POINT('Ctrl Pts',(1.42635858934674,20.3943871107668,13.));
#16293=CARTESIAN_POINT('Ctrl Pts',(1.38911568504378,20.5014457348136,13.));
#16294=CARTESIAN_POINT('Ctrl Pts',(1.34943433501682,20.6082844520171,13.));
#16295=CARTESIAN_POINT('Ctrl Pts',(1.30744723528262,20.7148563914567,13.));
#16296=CARTESIAN_POINT('Ctrl Pts',(1.27001463638626,20.8098680661832,13.));
#16297=CARTESIAN_POINT('Ctrl Pts',(1.23075788114852,20.9046675819449,13.));
#16298=CARTESIAN_POINT('Ctrl Pts',(1.18977154286166,20.9992246138384,13.));
#16299=CARTESIAN_POINT('Ctrl Pts',(1.13168263040835,21.1332379308873,13.));
#16300=CARTESIAN_POINT('Ctrl Pts',(1.07011397731129,21.2667633190311,13.));
#16301=CARTESIAN_POINT('Ctrl Pts',(1.00527632077043,21.399720077481,13.));
#16302=CARTESIAN_POINT('Ctrl Pts',(0.954911969009935,21.5029977298323,13.));
#16303=CARTESIAN_POINT('Ctrl Pts',(0.902570955775857,21.6059349889335,13.));
#16304=CARTESIAN_POINT('Ctrl Pts',(0.848338494937178,21.7084903365992,13.));
#16305=CARTESIAN_POINT('Ctrl Pts',(0.801423318189067,21.7972084620133,13.));
#16306=CARTESIAN_POINT('Ctrl Pts',(0.753096148369746,21.8856382920406,13.));
#16307=CARTESIAN_POINT('Ctrl Pts',(0.703383282930066,21.9737740846455,13.));
#16308=CARTESIAN_POINT('Ctrl Pts',(0.700514964692425,21.9788593175944,13.));
#16309=CARTESIAN_POINT('Ctrl Pts',(0.697642020369455,21.9839435768553,13.));
#16310=CARTESIAN_POINT('Ctrl Pts',(0.694764450219583,21.9890268624765,13.));
#16311=CARTESIAN_POINT('Ctrl Pts',(6.13422273260091,21.1275013067528,0.));
#16312=CARTESIAN_POINT('Ctrl Pts',(6.13422273260091,21.1275013067528,21.));
#16313=CARTESIAN_POINT('Ctrl Pts',(6.12649903511518,21.1204271980506,0.));
#16314=CARTESIAN_POINT('Ctrl Pts',(6.12649903511518,21.1204271980506,21.));
#16315=CARTESIAN_POINT('Ctrl Pts',(6.11107360216958,21.1062663590356,0.));
#16316=CARTESIAN_POINT('Ctrl Pts',(6.11107360216958,21.1062663590356,21.));
#16317=CARTESIAN_POINT('Ctrl Pts',(6.08800133883115,21.0849872356853,0.));
#16318=CARTESIAN_POINT('Ctrl Pts',(6.08800133883115,21.0849872356853,21.));
#16319=CARTESIAN_POINT('Ctrl Pts',(6.05737013696533,21.0565393163693,0.));
#16320=CARTESIAN_POINT('Ctrl Pts',(6.05737013696533,21.0565393163693,21.));
#16321=CARTESIAN_POINT('Ctrl Pts',(6.01930117633045,21.0208530236003,0.));
#16322=CARTESIAN_POINT('Ctrl Pts',(6.01930117633045,21.0208530236003,21.));
#16323=CARTESIAN_POINT('Ctrl Pts',(5.98145286361837,20.9850401822713,0.));
#16324=CARTESIAN_POINT('Ctrl Pts',(5.98145286361837,20.9850401822713,21.));
#16325=CARTESIAN_POINT('Ctrl Pts',(5.94382608200804,20.9491006734021,0.));
#16326=CARTESIAN_POINT('Ctrl Pts',(5.94382608200804,20.9491006734021,21.));
#16327=CARTESIAN_POINT('Ctrl Pts',(5.906422006626,20.9130344665641,0.));
#16328=CARTESIAN_POINT('Ctrl Pts',(5.906422006626,20.9130344665641,21.));
#16329=CARTESIAN_POINT('Ctrl Pts',(5.86924212736288,20.8768416821402,0.));
#16330=CARTESIAN_POINT('Ctrl Pts',(5.86924212736288,20.8768416821402,21.));
#16331=CARTESIAN_POINT('Ctrl Pts',(5.83228817460178,20.8405225541277,0.));
#16332=CARTESIAN_POINT('Ctrl Pts',(5.83228817460178,20.8405225541277,21.));
#16333=CARTESIAN_POINT('Ctrl Pts',(5.79556203439644,20.8040773827343,0.));
#16334=CARTESIAN_POINT('Ctrl Pts',(5.79556203439644,20.8040773827343,21.));
#16335=CARTESIAN_POINT('Ctrl Pts',(5.75906566327796,20.7675064905026,0.));
#16336=CARTESIAN_POINT('Ctrl Pts',(5.75906566327796,20.7675064905026,21.));
#16337=CARTESIAN_POINT('Ctrl Pts',(5.72280100798241,20.7308101804425,0.));
#16338=CARTESIAN_POINT('Ctrl Pts',(5.72280100798241,20.7308101804425,21.));
#16339=CARTESIAN_POINT('Ctrl Pts',(5.68676990500163,20.6939886877061,0.));
#16340=CARTESIAN_POINT('Ctrl Pts',(5.68676990500163,20.6939886877061,21.));
#16341=CARTESIAN_POINT('Ctrl Pts',(5.65097411164335,20.6570421847033,0.));
#16342=CARTESIAN_POINT('Ctrl Pts',(5.65097411164335,20.6570421847033,21.));
#16343=CARTESIAN_POINT('Ctrl Pts',(5.61541536715149,20.6199707996366,0.));
#16344=CARTESIAN_POINT('Ctrl Pts',(5.61541536715149,20.6199707996366,21.));
#16345=CARTESIAN_POINT('Ctrl Pts',(5.58009544402475,20.5827746317185,0.));
#16346=CARTESIAN_POINT('Ctrl Pts',(5.58009544402475,20.5827746317185,21.));
#16347=CARTESIAN_POINT('Ctrl Pts',(5.5450161968946,20.5454537676144,0.));
#16348=CARTESIAN_POINT('Ctrl Pts',(5.5450161968946,20.5454537676144,21.));
#16349=CARTESIAN_POINT('Ctrl Pts',(5.51017962306782,20.5080083009242,0.));
#16350=CARTESIAN_POINT('Ctrl Pts',(5.51017962306782,20.5080083009242,21.));
#16351=CARTESIAN_POINT('Ctrl Pts',(5.47558784449851,20.4704383353718,0.));
#16352=CARTESIAN_POINT('Ctrl Pts',(5.47558784449851,20.4704383353718,21.));
#16353=CARTESIAN_POINT('Ctrl Pts',(5.44124306065111,20.4327439816542,0.));
#16354=CARTESIAN_POINT('Ctrl Pts',(5.44124306065111,20.4327439816542,21.));
#16355=CARTESIAN_POINT('Ctrl Pts',(5.40714750595875,20.3949253578015,0.));
#16356=CARTESIAN_POINT('Ctrl Pts',(5.40714750595875,20.3949253578015,21.));
#16357=CARTESIAN_POINT('Ctrl Pts',(5.37330341114649,20.3569825877537,0.));
#16358=CARTESIAN_POINT('Ctrl Pts',(5.37330341114649,20.3569825877537,21.));
#16359=CARTESIAN_POINT('Ctrl Pts',(5.33971294212214,20.3189158047642,0.));
#16360=CARTESIAN_POINT('Ctrl Pts',(5.33971294212214,20.3189158047642,21.));
#16361=CARTESIAN_POINT('Ctrl Pts',(5.30637824220998,20.2807251380077,0.));
#16362=CARTESIAN_POINT('Ctrl Pts',(5.30637824220998,20.2807251380077,21.));
#16363=CARTESIAN_POINT('Ctrl Pts',(5.2733015229815,20.2424106921768,0.));
#16364=CARTESIAN_POINT('Ctrl Pts',(5.2733015229815,20.2424106921768,21.));
#16365=CARTESIAN_POINT('Ctrl Pts',(5.24048514441891,20.2039725283917,0.));
#16366=CARTESIAN_POINT('Ctrl Pts',(5.24048514441891,20.2039725283917,21.));
#16367=CARTESIAN_POINT('Ctrl Pts',(5.20793168386164,20.1654106491899,0.));
#16368=CARTESIAN_POINT('Ctrl Pts',(5.20793168386164,20.1654106491899,21.));
#16369=CARTESIAN_POINT('Ctrl Pts',(5.17564404279922,20.1267249732337,0.));
#16370=CARTESIAN_POINT('Ctrl Pts',(5.17564404279922,20.1267249732337,21.));
#16371=CARTESIAN_POINT('Ctrl Pts',(5.14362537555398,20.087915358486,0.));
#16372=CARTESIAN_POINT('Ctrl Pts',(5.14362537555398,20.087915358486,21.));
#16373=CARTESIAN_POINT('Ctrl Pts',(5.11187891582335,20.0489816528155,0.));
#16374=CARTESIAN_POINT('Ctrl Pts',(5.11187891582335,20.0489816528155,21.));
#16375=CARTESIAN_POINT('Ctrl Pts',(5.08040781745337,20.0099237417206,0.));
#16376=CARTESIAN_POINT('Ctrl Pts',(5.08040781745337,20.0099237417206,21.));
#16377=CARTESIAN_POINT('Ctrl Pts',(5.04921502064063,19.9707415879783,0.));
#16378=CARTESIAN_POINT('Ctrl Pts',(5.04921502064063,19.9707415879783,21.));
#16379=CARTESIAN_POINT('Ctrl Pts',(5.01830302225557,19.931435301086,0.));
#16380=CARTESIAN_POINT('Ctrl Pts',(5.01830302225557,19.931435301086,21.));
#16381=CARTESIAN_POINT('Ctrl Pts',(4.98767405031333,19.8920050831202,0.));
#16382=CARTESIAN_POINT('Ctrl Pts',(4.98767405031333,19.8920050831202,21.));
#16383=CARTESIAN_POINT('Ctrl Pts',(4.95733049830096,19.8524510953961,0.));
#16384=CARTESIAN_POINT('Ctrl Pts',(4.95733049830096,19.8524510953961,21.));
#16385=CARTESIAN_POINT('Ctrl Pts',(4.92727531494347,19.8127733387903,0.));
#16386=CARTESIAN_POINT('Ctrl Pts',(4.92727531494347,19.8127733387903,21.));
#16387=CARTESIAN_POINT('Ctrl Pts',(4.89751233527805,19.772971552601,0.));
#16388=CARTESIAN_POINT('Ctrl Pts',(4.89751233527805,19.772971552601,21.));
#16389=CARTESIAN_POINT('Ctrl Pts',(4.86804682289087,19.7330450480715,0.));
#16390=CARTESIAN_POINT('Ctrl Pts',(4.86804682289087,19.7330450480715,21.));
#16391=CARTESIAN_POINT('Ctrl Pts',(4.83888510708974,19.6929928227072,0.));
#16392=CARTESIAN_POINT('Ctrl Pts',(4.83888510708974,19.6929928227072,21.));
#16393=CARTESIAN_POINT('Ctrl Pts',(4.81003361418061,19.6528138625329,0.));
#16394=CARTESIAN_POINT('Ctrl Pts',(4.81003361418061,19.6528138625329,21.));
#16395=CARTESIAN_POINT('Ctrl Pts',(4.7814979936173,19.6125074152527,0.));
#16396=CARTESIAN_POINT('Ctrl Pts',(4.7814979936173,19.6125074152527,21.));
#16397=CARTESIAN_POINT('Ctrl Pts',(4.75328238194611,19.5720732205813,0.));
#16398=CARTESIAN_POINT('Ctrl Pts',(4.75328238194611,19.5720732205813,21.));
#16399=CARTESIAN_POINT('Ctrl Pts',(4.72538815796616,19.531511899192,0.));
#16400=CARTESIAN_POINT('Ctrl Pts',(4.72538815796616,19.531511899192,21.));
#16401=CARTESIAN_POINT('Ctrl Pts',(4.69781487613784,19.4908246636763,0.));
#16402=CARTESIAN_POINT('Ctrl Pts',(4.69781487613784,19.4908246636763,21.));
#16403=CARTESIAN_POINT('Ctrl Pts',(4.67056260851453,19.4500125912299,0.));
#16404=CARTESIAN_POINT('Ctrl Pts',(4.67056260851453,19.4500125912299,21.));
#16405=CARTESIAN_POINT('Ctrl Pts',(4.64363405547472,19.4090759683639,0.));
#16406=CARTESIAN_POINT('Ctrl Pts',(4.64363405547472,19.4090759683639,21.));
#16407=CARTESIAN_POINT('Ctrl Pts',(4.61703633725712,19.3680137353983,0.));
#16408=CARTESIAN_POINT('Ctrl Pts',(4.61703633725712,19.3680137353983,21.));
#16409=CARTESIAN_POINT('Ctrl Pts',(4.59078395765677,19.3268225655679,0.));
#16410=CARTESIAN_POINT('Ctrl Pts',(4.59078395765677,19.3268225655679,21.));
#16411=CARTESIAN_POINT('Ctrl Pts',(4.56489651606741,19.2854975819105,0.));
#16412=CARTESIAN_POINT('Ctrl Pts',(4.56489651606741,19.2854975819105,21.));
#16413=CARTESIAN_POINT('Ctrl Pts',(4.53939338835152,19.2440340196551,0.));
#16414=CARTESIAN_POINT('Ctrl Pts',(4.53939338835152,19.2440340196551,21.));
#16415=CARTESIAN_POINT('Ctrl Pts',(4.51428889122955,19.2024287376926,0.));
#16416=CARTESIAN_POINT('Ctrl Pts',(4.51428889122955,19.2024287376926,21.));
#16417=CARTESIAN_POINT('Ctrl Pts',(4.48958819710577,19.1606814968494,0.));
#16418=CARTESIAN_POINT('Ctrl Pts',(4.48958819710577,19.1606814968494,21.));
#16419=CARTESIAN_POINT('Ctrl Pts',(4.46528051067021,19.1187970904933,0.));
#16420=CARTESIAN_POINT('Ctrl Pts',(4.46528051067021,19.1187970904933,21.));
#16421=CARTESIAN_POINT('Ctrl Pts',(4.44134542994082,19.0767833717249,0.));
#16422=CARTESIAN_POINT('Ctrl Pts',(4.44134542994082,19.0767833717249,21.));
#16423=CARTESIAN_POINT('Ctrl Pts',(4.41776558033332,19.034647328575,0.));
#16424=CARTESIAN_POINT('Ctrl Pts',(4.41776558033332,19.034647328575,21.));
#16425=CARTESIAN_POINT('Ctrl Pts',(4.39453820875555,18.9923914823906,0.));
#16426=CARTESIAN_POINT('Ctrl Pts',(4.39453820875555,18.9923914823906,21.));
#16427=CARTESIAN_POINT('Ctrl Pts',(4.37168516143123,18.9500107909187,0.));
#16428=CARTESIAN_POINT('Ctrl Pts',(4.37168516143123,18.9500107909187,21.));
#16429=CARTESIAN_POINT('Ctrl Pts',(4.34926881342022,18.9074876952706,0.));
#16430=CARTESIAN_POINT('Ctrl Pts',(4.34926881342022,18.9074876952706,21.));
#16431=CARTESIAN_POINT('Ctrl Pts',(4.32737526247704,18.8647973781745,0.));
#16432=CARTESIAN_POINT('Ctrl Pts',(4.32737526247704,18.8647973781745,21.));
#16433=CARTESIAN_POINT('Ctrl Pts',(4.30608591031526,18.8219166495975,0.));
#16434=CARTESIAN_POINT('Ctrl Pts',(4.30608591031526,18.8219166495975,21.));
#16435=CARTESIAN_POINT('Ctrl Pts',(4.28545098663153,18.778832216358,0.));
#16436=CARTESIAN_POINT('Ctrl Pts',(4.28545098663153,18.778832216358,21.));
#16437=CARTESIAN_POINT('Ctrl Pts',(4.26546636161933,18.735547949685,0.));
#16438=CARTESIAN_POINT('Ctrl Pts',(4.26546636161933,18.735547949685,21.));
#16439=CARTESIAN_POINT('Ctrl Pts',(4.24603817988452,18.6920958920047,0.));
#16440=CARTESIAN_POINT('Ctrl Pts',(4.24603817988452,18.6920958920047,21.));
#16441=CARTESIAN_POINT('Ctrl Pts',(4.22703266508919,18.6485210883348,0.));
#16442=CARTESIAN_POINT('Ctrl Pts',(4.22703266508919,18.6485210883348,21.));
#16443=CARTESIAN_POINT('Ctrl Pts',(4.20834600700665,18.6048602364653,0.));
#16444=CARTESIAN_POINT('Ctrl Pts',(4.20834600700665,18.6048602364653,21.));
#16445=CARTESIAN_POINT('Ctrl Pts',(4.18996967278621,18.5611217636409,0.));
#16446=CARTESIAN_POINT('Ctrl Pts',(4.18996967278621,18.5611217636409,21.));
#16447=CARTESIAN_POINT('Ctrl Pts',(4.17205262766562,18.5172668097744,0.));
#16448=CARTESIAN_POINT('Ctrl Pts',(4.17205262766562,18.5172668097744,21.));
#16449=CARTESIAN_POINT('Ctrl Pts',(4.15497867673974,18.4731856794913,0.));
#16450=CARTESIAN_POINT('Ctrl Pts',(4.15497867673974,18.4731856794913,21.));
#16451=CARTESIAN_POINT('Ctrl Pts',(4.13926275457062,18.4287286547442,0.));
#16452=CARTESIAN_POINT('Ctrl Pts',(4.13926275457062,18.4287286547442,21.));
#16453=CARTESIAN_POINT('Ctrl Pts',(4.12819301671079,18.3927403741815,0.));
#16454=CARTESIAN_POINT('Ctrl Pts',(4.12819301671079,18.3927403741815,21.));
#16455=CARTESIAN_POINT('Ctrl Pts',(4.1209201986886,18.3654573320481,0.));
#16456=CARTESIAN_POINT('Ctrl Pts',(4.1209201986886,18.3654573320481,21.));
#16457=CARTESIAN_POINT('Ctrl Pts',(4.11655269114951,18.3471320125699,0.));
#16458=CARTESIAN_POINT('Ctrl Pts',(4.11655269114951,18.3471320125699,21.));
#16459=CARTESIAN_POINT('Ctrl Pts',(4.11448919812531,18.337935196262,0.));
#16460=CARTESIAN_POINT('Ctrl Pts',(4.11448919812531,18.337935196262,21.));
#16461=CARTESIAN_POINT('',(6.13422273260085,21.1275013067529,0.));
#16462=CARTESIAN_POINT('Ctrl Pts',(4.11448919812531,18.337935196262,0.));
#16463=CARTESIAN_POINT('Ctrl Pts',(4.11655269114951,18.3471320125699,0.));
#16464=CARTESIAN_POINT('Ctrl Pts',(4.1209201986886,18.3654573320481,0.));
#16465=CARTESIAN_POINT('Ctrl Pts',(4.12819301671079,18.3927403741815,0.));
#16466=CARTESIAN_POINT('Ctrl Pts',(4.13926275457062,18.4287286547442,0.));
#16467=CARTESIAN_POINT('Ctrl Pts',(4.15497867673974,18.4731856794913,0.));
#16468=CARTESIAN_POINT('Ctrl Pts',(4.17205262766562,18.5172668097744,0.));
#16469=CARTESIAN_POINT('Ctrl Pts',(4.18996967278621,18.5611217636409,0.));
#16470=CARTESIAN_POINT('Ctrl Pts',(4.20834600700665,18.6048602364653,0.));
#16471=CARTESIAN_POINT('Ctrl Pts',(4.22703266508919,18.6485210883348,0.));
#16472=CARTESIAN_POINT('Ctrl Pts',(4.24603817988452,18.6920958920047,0.));
#16473=CARTESIAN_POINT('Ctrl Pts',(4.26546636161933,18.735547949685,0.));
#16474=CARTESIAN_POINT('Ctrl Pts',(4.28545098663153,18.778832216358,0.));
#16475=CARTESIAN_POINT('Ctrl Pts',(4.30608591031526,18.8219166495975,0.));
#16476=CARTESIAN_POINT('Ctrl Pts',(4.32737526247704,18.8647973781745,0.));
#16477=CARTESIAN_POINT('Ctrl Pts',(4.34926881342022,18.9074876952706,0.));
#16478=CARTESIAN_POINT('Ctrl Pts',(4.37168516143123,18.9500107909187,0.));
#16479=CARTESIAN_POINT('Ctrl Pts',(4.39453820875555,18.9923914823906,0.));
#16480=CARTESIAN_POINT('Ctrl Pts',(4.41776558033332,19.034647328575,0.));
#16481=CARTESIAN_POINT('Ctrl Pts',(4.44134542994082,19.0767833717249,0.));
#16482=CARTESIAN_POINT('Ctrl Pts',(4.46528051067021,19.1187970904933,0.));
#16483=CARTESIAN_POINT('Ctrl Pts',(4.48958819710577,19.1606814968494,0.));
#16484=CARTESIAN_POINT('Ctrl Pts',(4.51428889122955,19.2024287376926,0.));
#16485=CARTESIAN_POINT('Ctrl Pts',(4.53939338835152,19.2440340196551,0.));
#16486=CARTESIAN_POINT('Ctrl Pts',(4.56489651606741,19.2854975819105,0.));
#16487=CARTESIAN_POINT('Ctrl Pts',(4.59078395765677,19.3268225655679,0.));
#16488=CARTESIAN_POINT('Ctrl Pts',(4.61703633725712,19.3680137353983,0.));
#16489=CARTESIAN_POINT('Ctrl Pts',(4.64363405547472,19.4090759683639,0.));
#16490=CARTESIAN_POINT('Ctrl Pts',(4.67056260851453,19.4500125912299,0.));
#16491=CARTESIAN_POINT('Ctrl Pts',(4.69781487613784,19.4908246636763,0.));
#16492=CARTESIAN_POINT('Ctrl Pts',(4.72538815796616,19.531511899192,0.));
#16493=CARTESIAN_POINT('Ctrl Pts',(4.75328238194611,19.5720732205813,0.));
#16494=CARTESIAN_POINT('Ctrl Pts',(4.7814979936173,19.6125074152527,0.));
#16495=CARTESIAN_POINT('Ctrl Pts',(4.81003361418061,19.6528138625329,0.));
#16496=CARTESIAN_POINT('Ctrl Pts',(4.83888510708974,19.6929928227072,0.));
#16497=CARTESIAN_POINT('Ctrl Pts',(4.86804682289087,19.7330450480715,0.));
#16498=CARTESIAN_POINT('Ctrl Pts',(4.89751233527805,19.772971552601,0.));
#16499=CARTESIAN_POINT('Ctrl Pts',(4.92727531494347,19.8127733387903,0.));
#16500=CARTESIAN_POINT('Ctrl Pts',(4.95733049830096,19.8524510953961,0.));
#16501=CARTESIAN_POINT('Ctrl Pts',(4.98767405031333,19.8920050831202,0.));
#16502=CARTESIAN_POINT('Ctrl Pts',(5.01830302225557,19.931435301086,0.));
#16503=CARTESIAN_POINT('Ctrl Pts',(5.04921502064063,19.9707415879783,0.));
#16504=CARTESIAN_POINT('Ctrl Pts',(5.08040781745337,20.0099237417206,0.));
#16505=CARTESIAN_POINT('Ctrl Pts',(5.11187891582335,20.0489816528155,0.));
#16506=CARTESIAN_POINT('Ctrl Pts',(5.14362537555398,20.087915358486,0.));
#16507=CARTESIAN_POINT('Ctrl Pts',(5.17564404279922,20.1267249732337,0.));
#16508=CARTESIAN_POINT('Ctrl Pts',(5.20793168386164,20.1654106491899,0.));
#16509=CARTESIAN_POINT('Ctrl Pts',(5.24048514441891,20.2039725283917,0.));
#16510=CARTESIAN_POINT('Ctrl Pts',(5.2733015229815,20.2424106921768,0.));
#16511=CARTESIAN_POINT('Ctrl Pts',(5.30637824220998,20.2807251380077,0.));
#16512=CARTESIAN_POINT('Ctrl Pts',(5.33971294212214,20.3189158047642,0.));
#16513=CARTESIAN_POINT('Ctrl Pts',(5.37330341114649,20.3569825877537,0.));
#16514=CARTESIAN_POINT('Ctrl Pts',(5.40714750595875,20.3949253578015,0.));
#16515=CARTESIAN_POINT('Ctrl Pts',(5.44124306065111,20.4327439816542,0.));
#16516=CARTESIAN_POINT('Ctrl Pts',(5.47558784449851,20.4704383353718,0.));
#16517=CARTESIAN_POINT('Ctrl Pts',(5.51017962306782,20.5080083009242,0.));
#16518=CARTESIAN_POINT('Ctrl Pts',(5.5450161968946,20.5454537676144,0.));
#16519=CARTESIAN_POINT('Ctrl Pts',(5.58009544402475,20.5827746317185,0.));
#16520=CARTESIAN_POINT('Ctrl Pts',(5.61541536715149,20.6199707996366,0.));
#16521=CARTESIAN_POINT('Ctrl Pts',(5.65097411164335,20.6570421847033,0.));
#16522=CARTESIAN_POINT('Ctrl Pts',(5.68676990500163,20.6939886877061,0.));
#16523=CARTESIAN_POINT('Ctrl Pts',(5.72280100798241,20.7308101804425,0.));
#16524=CARTESIAN_POINT('Ctrl Pts',(5.75906566327796,20.7675064905026,0.));
#16525=CARTESIAN_POINT('Ctrl Pts',(5.79556203439644,20.8040773827343,0.));
#16526=CARTESIAN_POINT('Ctrl Pts',(5.83228817460178,20.8405225541277,0.));
#16527=CARTESIAN_POINT('Ctrl Pts',(5.86924212736288,20.8768416821402,0.));
#16528=CARTESIAN_POINT('Ctrl Pts',(5.906422006626,20.9130344665641,0.));
#16529=CARTESIAN_POINT('Ctrl Pts',(5.94382608200804,20.9491006734021,0.));
#16530=CARTESIAN_POINT('Ctrl Pts',(5.98145286361837,20.9850401822713,0.));
#16531=CARTESIAN_POINT('Ctrl Pts',(6.02687083887287,21.0280155918661,0.));
#16532=CARTESIAN_POINT('Ctrl Pts',(6.06499496148845,21.0636702474951,0.));
#16533=CARTESIAN_POINT('Ctrl Pts',(6.09567013127872,21.0920928984154,0.));
#16534=CARTESIAN_POINT('Ctrl Pts',(6.11877533761501,21.1133530893457,0.));
#16535=CARTESIAN_POINT('Ctrl Pts',(6.13422273260091,21.1275013067528,0.));
#16536=CARTESIAN_POINT('',(6.13422273260085,21.1275013067529,13.));
#16537=CARTESIAN_POINT('Ctrl Pts',(6.13422273260091,21.1275013067528,13.));
#16538=CARTESIAN_POINT('Ctrl Pts',(6.05818207473574,21.0578559224639,13.));
#16539=CARTESIAN_POINT('Ctrl Pts',(5.98341417184728,20.9874765040291,13.));
#16540=CARTESIAN_POINT('Ctrl Pts',(5.90994468705573,20.9163599154701,13.));
#16541=CARTESIAN_POINT('Ctrl Pts',(5.78820256793375,20.7985166473367,13.));
#16542=CARTESIAN_POINT('Ctrl Pts',(5.67003811891006,20.6786545089329,13.));
#16543=CARTESIAN_POINT('Ctrl Pts',(5.55573863837942,20.5568062999927,13.));
#16544=CARTESIAN_POINT('Ctrl Pts',(5.46788135576792,20.4631466221109,13.));
#16545=CARTESIAN_POINT('Ctrl Pts',(5.38230707228741,20.3683108766733,13.));
#16546=CARTESIAN_POINT('Ctrl Pts',(5.29917141508608,20.2723075580748,13.));
#16547=CARTESIAN_POINT('Ctrl Pts',(5.20967788534761,20.1689623012113,13.));
#16548=CARTESIAN_POINT('Ctrl Pts',(5.12300395967644,20.064265111617,13.));
#16549=CARTESIAN_POINT('Ctrl Pts',(5.03941267492058,19.9582092059413,13.));
#16550=CARTESIAN_POINT('Ctrl Pts',(4.9931342664069,19.8994937723589,13.));
#16551=CARTESIAN_POINT('Ctrl Pts',(4.94779583855815,19.8403635590138,13.));
#16552=CARTESIAN_POINT('Ctrl Pts',(4.90344584338495,19.7808173191098,13.));
#16553=CARTESIAN_POINT('Ctrl Pts',(4.86070845303356,19.7234362328482,13.));
#16554=CARTESIAN_POINT('Ctrl Pts',(4.81889538663267,19.6656667932077,13.));
#16555=CARTESIAN_POINT('Ctrl Pts',(4.77808296591823,19.6074986363137,13.));
#16556=CARTESIAN_POINT('Ctrl Pts',(4.74280851516602,19.5572235056112,13.));
#16557=CARTESIAN_POINT('Ctrl Pts',(4.70827845343013,19.5066514996463,13.));
#16558=CARTESIAN_POINT('Ctrl Pts',(4.67449772183394,19.4557905178253,13.));
#16559=CARTESIAN_POINT('Ctrl Pts',(4.65025481932131,19.4192898925955,13.));
#16560=CARTESIAN_POINT('Ctrl Pts',(4.62639514873701,19.3826412892821,13.));
#16561=CARTESIAN_POINT('Ctrl Pts',(4.60295743098886,19.3458364388947,13.));
#16562=CARTESIAN_POINT('Ctrl Pts',(4.57990136672579,19.309630908781,13.));
#16563=CARTESIAN_POINT('Ctrl Pts',(4.55725972003952,19.2732722738433,13.));
#16564=CARTESIAN_POINT('Ctrl Pts',(4.53508357570349,19.2367485577747,13.));
#16565=CARTESIAN_POINT('Ctrl Pts',(4.51585555588996,19.2050803504619,13.));
#16566=CARTESIAN_POINT('Ctrl Pts',(4.49697986260364,19.1732873013817,13.));
#16567=CARTESIAN_POINT('Ctrl Pts',(4.47844262266263,19.1413765621746,13.));
#16568=CARTESIAN_POINT('Ctrl Pts',(4.46165213672774,19.1124727545132,13.));
#16569=CARTESIAN_POINT('Ctrl Pts',(4.44513401132745,19.0834740457553,13.));
#16570=CARTESIAN_POINT('Ctrl Pts',(4.42886646477444,19.0543895553857,13.));
#16571=CARTESIAN_POINT('Ctrl Pts',(4.41516354273523,19.0298903168075,13.));
#16572=CARTESIAN_POINT('Ctrl Pts',(4.4016367609421,19.0053307307673,13.));
#16573=CARTESIAN_POINT('Ctrl Pts',(4.3883055171539,18.9807063065615,13.));
#16574=CARTESIAN_POINT('Ctrl Pts',(4.36901375650801,18.9450720847762,13.));
#16575=CARTESIAN_POINT('Ctrl Pts',(4.35013223001517,18.9093017976082,13.));
#16576=CARTESIAN_POINT('Ctrl Pts',(4.33187128665099,18.8733353263476,13.));
#16577=CARTESIAN_POINT('Ctrl Pts',(4.32083731650082,18.8516029896122,13.));
#16578=CARTESIAN_POINT('Ctrl Pts',(4.31003325580781,18.8297980041067,13.));
#16579=CARTESIAN_POINT('Ctrl Pts',(4.29948469299916,18.8079138028469,13.));
#16580=CARTESIAN_POINT('Ctrl Pts',(4.28975595055798,18.7877304128013,13.));
#16581=CARTESIAN_POINT('Ctrl Pts',(4.2802457999774,18.7674792480964,13.));
#16582=CARTESIAN_POINT('Ctrl Pts',(4.27093067973601,18.7471689056956,13.));
#16583=CARTESIAN_POINT('Ctrl Pts',(4.25811678806992,18.7192299719535,13.));
#16584=CARTESIAN_POINT('Ctrl Pts',(4.24566493397902,18.6911811213441,13.));
#16585=CARTESIAN_POINT('Ctrl Pts',(4.23343245343651,18.66307117359,13.));
#16586=CARTESIAN_POINT('Ctrl Pts',(4.22567194943085,18.6452377209729,13.));
#16587=CARTESIAN_POINT('Ctrl Pts',(4.21799814921963,18.6273802008541,13.));
#16588=CARTESIAN_POINT('Ctrl Pts',(4.21040342108918,18.6095026819599,13.));
#16589=CARTESIAN_POINT('Ctrl Pts',(4.20358750609861,18.5934584408847,13.));
#16590=CARTESIAN_POINT('Ctrl Pts',(4.19683458198288,18.5773983085052,13.));
#16591=CARTESIAN_POINT('Ctrl Pts',(4.19017810368263,18.561313537851,13.));
#16592=CARTESIAN_POINT('Ctrl Pts',(4.18318081928036,18.5444052404397,13.));
#16593=CARTESIAN_POINT('Ctrl Pts',(4.17628995976728,18.5274697699695,13.));
#16594=CARTESIAN_POINT('Ctrl Pts',(4.16960404102764,18.5104789585715,13.));
#16595=CARTESIAN_POINT('Ctrl Pts',(4.15849874476065,18.4822572583475,13.));
#16596=CARTESIAN_POINT('Ctrl Pts',(4.14796697295334,18.4538805850238,13.));
#16597=CARTESIAN_POINT('Ctrl Pts',(4.13860964460812,18.4251735640121,13.));
#16598=CARTESIAN_POINT('Ctrl Pts',(4.1334496807422,18.4093434909769,13.));
#16599=CARTESIAN_POINT('Ctrl Pts',(4.12864814561696,18.3934125378817,13.));
#16600=CARTESIAN_POINT('Ctrl Pts',(4.12427889810931,18.3773590065429,13.));
#16601=CARTESIAN_POINT('Ctrl Pts',(4.12072474060618,18.3643002867611,13.));
#16602=CARTESIAN_POINT('Ctrl Pts',(4.11745655843541,18.3511604736782,13.));
#16603=CARTESIAN_POINT('Ctrl Pts',(4.11448919812531,18.337935196262,13.));
#16604=CARTESIAN_POINT('',(6.13422273260085,21.1275013067529,0.));
#16605=CARTESIAN_POINT('Origin',(1.75106900012182E-12,5.38923623413286E-12,
0.));
#16606=CARTESIAN_POINT('',(7.45574324794401,20.698113262342,0.));
#16607=CARTESIAN_POINT('Origin',(1.75106900012182E-12,5.38923623413286E-12,
0.));
#16608=CARTESIAN_POINT('',(7.45574324794401,20.698113262342,13.));
#16609=CARTESIAN_POINT('Origin',(1.75106900012182E-12,5.38923623413286E-12,
13.));
#16610=CARTESIAN_POINT('',(7.45574324794401,20.698113262342,0.));
#16611=CARTESIAN_POINT('Ctrl Pts',(7.45007618140239,17.2541372868972,0.));
#16612=CARTESIAN_POINT('Ctrl Pts',(7.45007618140239,17.2541372868972,21.));
#16613=CARTESIAN_POINT('Ctrl Pts',(7.45381253347183,17.2627905583523,0.));
#16614=CARTESIAN_POINT('Ctrl Pts',(7.45381253347183,17.2627905583523,21.));
#16615=CARTESIAN_POINT('Ctrl Pts',(7.46105049818251,17.2801832097582,0.));
#16616=CARTESIAN_POINT('Ctrl Pts',(7.46105049818251,17.2801832097582,21.));
#16617=CARTESIAN_POINT('Ctrl Pts',(7.4712032346092,17.3065305096784,0.));
#16618=CARTESIAN_POINT('Ctrl Pts',(7.4712032346092,17.3065305096784,21.));
#16619=CARTESIAN_POINT('Ctrl Pts',(7.48340100912745,17.3421522689127,0.));
#16620=CARTESIAN_POINT('Ctrl Pts',(7.48340100912745,17.3421522689127,21.));
#16621=CARTESIAN_POINT('Ctrl Pts',(7.49681774451751,17.3873563447297,0.));
#16622=CARTESIAN_POINT('Ctrl Pts',(7.49681774451751,17.3873563447297,21.));
#16623=CARTESIAN_POINT('Ctrl Pts',(7.50891486634214,17.4330545448126,0.));
#16624=CARTESIAN_POINT('Ctrl Pts',(7.50891486634214,17.4330545448126,21.));
#16625=CARTESIAN_POINT('Ctrl Pts',(7.52019696747329,17.4790653226646,0.));
#16626=CARTESIAN_POINT('Ctrl Pts',(7.52019696747329,17.4790653226646,21.));
#16627=CARTESIAN_POINT('Ctrl Pts',(7.53103903007864,17.5252518287336,0.));
#16628=CARTESIAN_POINT('Ctrl Pts',(7.53103903007864,17.5252518287336,21.));
#16629=CARTESIAN_POINT('Ctrl Pts',(7.54158441095317,17.5715579419204,0.));
#16630=CARTESIAN_POINT('Ctrl Pts',(7.54158441095317,17.5715579419204,21.));
#16631=CARTESIAN_POINT('Ctrl Pts',(7.55182125346564,17.6179818599248,0.));
#16632=CARTESIAN_POINT('Ctrl Pts',(7.55182125346564,17.6179818599248,21.));
#16633=CARTESIAN_POINT('Ctrl Pts',(7.56164400295863,17.6645549117314,0.));
#16634=CARTESIAN_POINT('Ctrl Pts',(7.56164400295863,17.6645549117314,21.));
#16635=CARTESIAN_POINT('Ctrl Pts',(7.57091795530423,17.7113192869136,0.));
#16636=CARTESIAN_POINT('Ctrl Pts',(7.57091795530423,17.7113192869136,21.));
#16637=CARTESIAN_POINT('Ctrl Pts',(7.57954834582804,17.7583042294209,0.));
#16638=CARTESIAN_POINT('Ctrl Pts',(7.57954834582804,17.7583042294209,21.));
#16639=CARTESIAN_POINT('Ctrl Pts',(7.58752955799499,17.8055090348024,0.));
#16640=CARTESIAN_POINT('Ctrl Pts',(7.58752955799499,17.8055090348024,21.));
#16641=CARTESIAN_POINT('Ctrl Pts',(7.59491004201956,17.8529149331931,0.));
#16642=CARTESIAN_POINT('Ctrl Pts',(7.59491004201956,17.8529149331931,21.));
#16643=CARTESIAN_POINT('Ctrl Pts',(7.60176928403058,17.900492838997,0.));
#16644=CARTESIAN_POINT('Ctrl Pts',(7.60176928403058,17.900492838997,21.));
#16645=CARTESIAN_POINT('Ctrl Pts',(7.60819152580111,17.9482122228183,0.));
#16646=CARTESIAN_POINT('Ctrl Pts',(7.60819152580111,17.9482122228183,21.));
#16647=CARTESIAN_POINT('Ctrl Pts',(7.61423755067038,17.9960506269561,0.));
#16648=CARTESIAN_POINT('Ctrl Pts',(7.61423755067038,17.9960506269561,21.));
#16649=CARTESIAN_POINT('Ctrl Pts',(7.61992799636654,18.0439992897906,0.));
#16650=CARTESIAN_POINT('Ctrl Pts',(7.61992799636654,18.0439992897906,21.));
#16651=CARTESIAN_POINT('Ctrl Pts',(7.62525915358074,18.0920577897363,0.));
#16652=CARTESIAN_POINT('Ctrl Pts',(7.62525915358074,18.0920577897363,21.));
#16653=CARTESIAN_POINT('Ctrl Pts',(7.63021285851762,18.1402306858819,0.));
#16654=CARTESIAN_POINT('Ctrl Pts',(7.63021285851762,18.1402306858819,21.));
#16655=CARTESIAN_POINT('Ctrl Pts',(7.63476798969017,18.1885236169197,0.));
#16656=CARTESIAN_POINT('Ctrl Pts',(7.63476798969017,18.1885236169197,21.));
#16657=CARTESIAN_POINT('Ctrl Pts',(7.63891299603827,18.2369390502576,0.));
#16658=CARTESIAN_POINT('Ctrl Pts',(7.63891299603827,18.2369390502576,21.));
#16659=CARTESIAN_POINT('Ctrl Pts',(7.6426522027076,18.2854741391282,0.));
#16660=CARTESIAN_POINT('Ctrl Pts',(7.6426522027076,18.2854741391282,21.));
#16661=CARTESIAN_POINT('Ctrl Pts',(7.64599903846601,18.3341230095852,0.));
#16662=CARTESIAN_POINT('Ctrl Pts',(7.64599903846601,18.3341230095852,21.));
#16663=CARTESIAN_POINT('Ctrl Pts',(7.6489719793775,18.3828781275628,0.));
#16664=CARTESIAN_POINT('Ctrl Pts',(7.6489719793775,18.3828781275628,21.));
#16665=CARTESIAN_POINT('Ctrl Pts',(7.65158974829126,18.4317319183719,0.));
#16666=CARTESIAN_POINT('Ctrl Pts',(7.65158974829126,18.4317319183719,21.));
#16667=CARTESIAN_POINT('Ctrl Pts',(7.65386603444743,18.4806785483052,0.));
#16668=CARTESIAN_POINT('Ctrl Pts',(7.65386603444743,18.4806785483052,21.));
#16669=CARTESIAN_POINT('Ctrl Pts',(7.65580722110437,18.5297146894905,0.));
#16670=CARTESIAN_POINT('Ctrl Pts',(7.65580722110437,18.5297146894905,21.));
#16671=CARTESIAN_POINT('Ctrl Pts',(7.65741532450727,18.5788385228928,0.));
#16672=CARTESIAN_POINT('Ctrl Pts',(7.65741532450727,18.5788385228928,21.));
#16673=CARTESIAN_POINT('Ctrl Pts',(7.65868976978872,18.6280491346907,0.));
#16674=CARTESIAN_POINT('Ctrl Pts',(7.65868976978872,18.6280491346907,21.));
#16675=CARTESIAN_POINT('Ctrl Pts',(7.65962948375621,18.6773458057584,0.));
#16676=CARTESIAN_POINT('Ctrl Pts',(7.65962948375621,18.6773458057584,21.));
#16677=CARTESIAN_POINT('Ctrl Pts',(7.66023521705905,18.7267272235231,0.));
#16678=CARTESIAN_POINT('Ctrl Pts',(7.66023521705905,18.7267272235231,21.));
#16679=CARTESIAN_POINT('Ctrl Pts',(7.66051046922541,18.7761911671591,0.));
#16680=CARTESIAN_POINT('Ctrl Pts',(7.66051046922541,18.7761911671591,21.));
#16681=CARTESIAN_POINT('Ctrl Pts',(7.66046025294775,18.8257349246207,0.));
#16682=CARTESIAN_POINT('Ctrl Pts',(7.66046025294775,18.8257349246207,21.));
#16683=CARTESIAN_POINT('Ctrl Pts',(7.66009036321663,18.8753555389435,0.));
#16684=CARTESIAN_POINT('Ctrl Pts',(7.66009036321663,18.8753555389435,21.));
#16685=CARTESIAN_POINT('Ctrl Pts',(7.65940650980099,18.9250501008887,0.));
#16686=CARTESIAN_POINT('Ctrl Pts',(7.65940650980099,18.9250501008887,21.));
#16687=CARTESIAN_POINT('Ctrl Pts',(7.65841335587266,18.974816073814,0.));
#16688=CARTESIAN_POINT('Ctrl Pts',(7.65841335587266,18.974816073814,21.));
#16689=CARTESIAN_POINT('Ctrl Pts',(7.65711415727855,19.0246514144531,0.));
#16690=CARTESIAN_POINT('Ctrl Pts',(7.65711415727855,19.0246514144531,21.));
#16691=CARTESIAN_POINT('Ctrl Pts',(7.65551129907202,19.0745543888799,0.));
#16692=CARTESIAN_POINT('Ctrl Pts',(7.65551129907202,19.0745543888799,21.));
#16693=CARTESIAN_POINT('Ctrl Pts',(7.65360662280609,19.1245234597312,0.));
#16694=CARTESIAN_POINT('Ctrl Pts',(7.65360662280609,19.1245234597312,21.));
#16695=CARTESIAN_POINT('Ctrl Pts',(7.65140181220526,19.1745571539291,0.));
#16696=CARTESIAN_POINT('Ctrl Pts',(7.65140181220526,19.1745571539291,21.));
#16697=CARTESIAN_POINT('Ctrl Pts',(7.64889882291924,19.224653915265,0.));
#16698=CARTESIAN_POINT('Ctrl Pts',(7.64889882291924,19.224653915265,21.));
#16699=CARTESIAN_POINT('Ctrl Pts',(7.64610005549614,19.2748120456486,0.));
#16700=CARTESIAN_POINT('Ctrl Pts',(7.64610005549614,19.2748120456486,21.));
#16701=CARTESIAN_POINT('Ctrl Pts',(7.64300812875339,19.3250297839295,0.));
#16702=CARTESIAN_POINT('Ctrl Pts',(7.64300812875339,19.3250297839295,21.));
#16703=CARTESIAN_POINT('Ctrl Pts',(7.63962574822761,19.3753053524647,0.));
#16704=CARTESIAN_POINT('Ctrl Pts',(7.63962574822761,19.3753053524647,21.));
#16705=CARTESIAN_POINT('Ctrl Pts',(7.63595554930654,19.4256370121006,0.));
#16706=CARTESIAN_POINT('Ctrl Pts',(7.63595554930654,19.4256370121006,21.));
#16707=CARTESIAN_POINT('Ctrl Pts',(7.63199992715366,19.4760231231881,0.));
#16708=CARTESIAN_POINT('Ctrl Pts',(7.63199992715366,19.4760231231881,21.));
#16709=CARTESIAN_POINT('Ctrl Pts',(7.62776096538883,19.5264621687521,0.));
#16710=CARTESIAN_POINT('Ctrl Pts',(7.62776096538883,19.5264621687521,21.));
#16711=CARTESIAN_POINT('Ctrl Pts',(7.6232405373522,19.5769527121826,0.));
#16712=CARTESIAN_POINT('Ctrl Pts',(7.6232405373522,19.5769527121826,21.));
#16713=CARTESIAN_POINT('Ctrl Pts',(7.61844037070591,19.6274933688524,0.));
#16714=CARTESIAN_POINT('Ctrl Pts',(7.61844037070591,19.6274933688524,21.));
#16715=CARTESIAN_POINT('Ctrl Pts',(7.61336212350879,19.6780827744426,0.));
#16716=CARTESIAN_POINT('Ctrl Pts',(7.61336212350879,19.6780827744426,21.));
#16717=CARTESIAN_POINT('Ctrl Pts',(7.60800746969262,19.7287195480601,0.));
#16718=CARTESIAN_POINT('Ctrl Pts',(7.60800746969262,19.7287195480601,21.));
#16719=CARTESIAN_POINT('Ctrl Pts',(7.60237814110187,19.7794022782484,0.));
#16720=CARTESIAN_POINT('Ctrl Pts',(7.60237814110187,19.7794022782484,21.));
#16721=CARTESIAN_POINT('Ctrl Pts',(7.59647587605448,19.830129556152,0.));
#16722=CARTESIAN_POINT('Ctrl Pts',(7.59647587605448,19.830129556152,21.));
#16723=CARTESIAN_POINT('Ctrl Pts',(7.59030238888852,19.8808999994024,0.));
#16724=CARTESIAN_POINT('Ctrl Pts',(7.59030238888852,19.8808999994024,21.));
#16725=CARTESIAN_POINT('Ctrl Pts',(7.58385933533352,19.931712276832,0.));
#16726=CARTESIAN_POINT('Ctrl Pts',(7.58385933533352,19.931712276832,21.));
#16727=CARTESIAN_POINT('Ctrl Pts',(7.57714827622806,19.9825651387294,0.));
#16728=CARTESIAN_POINT('Ctrl Pts',(7.57714827622806,19.9825651387294,21.));
#16729=CARTESIAN_POINT('Ctrl Pts',(7.57017066105973,20.0334574248557,0.));
#16730=CARTESIAN_POINT('Ctrl Pts',(7.57017066105973,20.0334574248557,21.));
#16731=CARTESIAN_POINT('Ctrl Pts',(7.5629278654946,20.0843880130978,0.));
#16732=CARTESIAN_POINT('Ctrl Pts',(7.5629278654946,20.0843880130978,21.));
#16733=CARTESIAN_POINT('Ctrl Pts',(7.55542122125495,20.1353557774357,0.));
#16734=CARTESIAN_POINT('Ctrl Pts',(7.55542122125495,20.1353557774357,21.));
#16735=CARTESIAN_POINT('Ctrl Pts',(7.54765204869254,20.1863595454674,0.));
#16736=CARTESIAN_POINT('Ctrl Pts',(7.54765204869254,20.1863595454674,21.));
#16737=CARTESIAN_POINT('Ctrl Pts',(7.53962169534167,20.2373980474879,0.));
#16738=CARTESIAN_POINT('Ctrl Pts',(7.53962169534167,20.2373980474879,21.));
#16739=CARTESIAN_POINT('Ctrl Pts',(7.53133155804008,20.2884698940944,0.));
#16740=CARTESIAN_POINT('Ctrl Pts',(7.53133155804008,20.2884698940944,21.));
#16741=CARTESIAN_POINT('Ctrl Pts',(7.52278303006887,20.3395736743243,0.));
#16742=CARTESIAN_POINT('Ctrl Pts',(7.52278303006887,20.3395736743243,21.));
#16743=CARTESIAN_POINT('Ctrl Pts',(7.51397746081994,20.3907080367098,0.));
#16744=CARTESIAN_POINT('Ctrl Pts',(7.51397746081994,20.3907080367098,21.));
#16745=CARTESIAN_POINT('Ctrl Pts',(7.50491611266253,20.4418717748497,0.));
#16746=CARTESIAN_POINT('Ctrl Pts',(7.50491611266253,20.4418717748497,21.));
#16747=CARTESIAN_POINT('Ctrl Pts',(7.49560012018406,20.4930639156161,0.));
#16748=CARTESIAN_POINT('Ctrl Pts',(7.49560012018406,20.4930639156161,21.));
#16749=CARTESIAN_POINT('Ctrl Pts',(7.48603045196745,20.5442837929044,0.));
#16750=CARTESIAN_POINT('Ctrl Pts',(7.48603045196745,20.5442837929044,21.));
#16751=CARTESIAN_POINT('Ctrl Pts',(7.47620789245428,20.5955309838521,0.));
#16752=CARTESIAN_POINT('Ctrl Pts',(7.47620789245428,20.5955309838521,21.));
#16753=CARTESIAN_POINT('Ctrl Pts',(7.46814799701906,20.6365504027501,0.));
#16754=CARTESIAN_POINT('Ctrl Pts',(7.46814799701906,20.6365504027501,21.));
#16755=CARTESIAN_POINT('Ctrl Pts',(7.46198969876654,20.6673271112931,0.));
#16756=CARTESIAN_POINT('Ctrl Pts',(7.46198969876654,20.6673271112931,21.));
#16757=CARTESIAN_POINT('Ctrl Pts',(7.45783379370108,20.6878503127065,0.));
#16758=CARTESIAN_POINT('Ctrl Pts',(7.45783379370108,20.6878503127065,21.));
#16759=CARTESIAN_POINT('Ctrl Pts',(7.45574324794401,20.698113262342,0.));
#16760=CARTESIAN_POINT('Ctrl Pts',(7.45574324794401,20.698113262342,21.));
#16761=CARTESIAN_POINT('Ctrl Pts',(7.45007618140239,17.2541372868972,0.));
#16762=CARTESIAN_POINT('Ctrl Pts',(7.45381253347183,17.2627905583523,0.));
#16763=CARTESIAN_POINT('Ctrl Pts',(7.46105049818251,17.2801832097582,0.));
#16764=CARTESIAN_POINT('Ctrl Pts',(7.4712032346092,17.3065305096784,0.));
#16765=CARTESIAN_POINT('Ctrl Pts',(7.48340100912745,17.3421522689127,0.));
#16766=CARTESIAN_POINT('Ctrl Pts',(7.49681774451751,17.3873563447297,0.));
#16767=CARTESIAN_POINT('Ctrl Pts',(7.50891486634214,17.4330545448126,0.));
#16768=CARTESIAN_POINT('Ctrl Pts',(7.52019696747329,17.4790653226646,0.));
#16769=CARTESIAN_POINT('Ctrl Pts',(7.53103903007864,17.5252518287336,0.));
#16770=CARTESIAN_POINT('Ctrl Pts',(7.54158441095317,17.5715579419204,0.));
#16771=CARTESIAN_POINT('Ctrl Pts',(7.55182125346564,17.6179818599248,0.));
#16772=CARTESIAN_POINT('Ctrl Pts',(7.56164400295863,17.6645549117314,0.));
#16773=CARTESIAN_POINT('Ctrl Pts',(7.57091795530423,17.7113192869136,0.));
#16774=CARTESIAN_POINT('Ctrl Pts',(7.57954834582804,17.7583042294209,0.));
#16775=CARTESIAN_POINT('Ctrl Pts',(7.58752955799499,17.8055090348024,0.));
#16776=CARTESIAN_POINT('Ctrl Pts',(7.59491004201956,17.8529149331931,0.));
#16777=CARTESIAN_POINT('Ctrl Pts',(7.60176928403058,17.900492838997,0.));
#16778=CARTESIAN_POINT('Ctrl Pts',(7.60819152580111,17.9482122228183,0.));
#16779=CARTESIAN_POINT('Ctrl Pts',(7.61423755067038,17.9960506269561,0.));
#16780=CARTESIAN_POINT('Ctrl Pts',(7.61992799636654,18.0439992897906,0.));
#16781=CARTESIAN_POINT('Ctrl Pts',(7.62525915358074,18.0920577897363,0.));
#16782=CARTESIAN_POINT('Ctrl Pts',(7.63021285851762,18.1402306858819,0.));
#16783=CARTESIAN_POINT('Ctrl Pts',(7.63476798969017,18.1885236169197,0.));
#16784=CARTESIAN_POINT('Ctrl Pts',(7.63891299603827,18.2369390502576,0.));
#16785=CARTESIAN_POINT('Ctrl Pts',(7.6426522027076,18.2854741391282,0.));
#16786=CARTESIAN_POINT('Ctrl Pts',(7.64599903846601,18.3341230095852,0.));
#16787=CARTESIAN_POINT('Ctrl Pts',(7.6489719793775,18.3828781275628,0.));
#16788=CARTESIAN_POINT('Ctrl Pts',(7.65158974829126,18.4317319183719,0.));
#16789=CARTESIAN_POINT('Ctrl Pts',(7.65386603444743,18.4806785483052,0.));
#16790=CARTESIAN_POINT('Ctrl Pts',(7.65580722110437,18.5297146894905,0.));
#16791=CARTESIAN_POINT('Ctrl Pts',(7.65741532450727,18.5788385228928,0.));
#16792=CARTESIAN_POINT('Ctrl Pts',(7.65868976978872,18.6280491346907,0.));
#16793=CARTESIAN_POINT('Ctrl Pts',(7.65962948375621,18.6773458057584,0.));
#16794=CARTESIAN_POINT('Ctrl Pts',(7.66023521705905,18.7267272235231,0.));
#16795=CARTESIAN_POINT('Ctrl Pts',(7.66051046922541,18.7761911671591,0.));
#16796=CARTESIAN_POINT('Ctrl Pts',(7.66046025294775,18.8257349246207,0.));
#16797=CARTESIAN_POINT('Ctrl Pts',(7.66009036321663,18.8753555389435,0.));
#16798=CARTESIAN_POINT('Ctrl Pts',(7.65940650980099,18.9250501008887,0.));
#16799=CARTESIAN_POINT('Ctrl Pts',(7.65841335587266,18.974816073814,0.));
#16800=CARTESIAN_POINT('Ctrl Pts',(7.65711415727855,19.0246514144531,0.));
#16801=CARTESIAN_POINT('Ctrl Pts',(7.65551129907202,19.0745543888799,0.));
#16802=CARTESIAN_POINT('Ctrl Pts',(7.65360662280609,19.1245234597312,0.));
#16803=CARTESIAN_POINT('Ctrl Pts',(7.65140181220526,19.1745571539291,0.));
#16804=CARTESIAN_POINT('Ctrl Pts',(7.64889882291924,19.224653915265,0.));
#16805=CARTESIAN_POINT('Ctrl Pts',(7.64610005549614,19.2748120456486,0.));
#16806=CARTESIAN_POINT('Ctrl Pts',(7.64300812875339,19.3250297839295,0.));
#16807=CARTESIAN_POINT('Ctrl Pts',(7.63962574822761,19.3753053524647,0.));
#16808=CARTESIAN_POINT('Ctrl Pts',(7.63595554930654,19.4256370121006,0.));
#16809=CARTESIAN_POINT('Ctrl Pts',(7.63199992715366,19.4760231231881,0.));
#16810=CARTESIAN_POINT('Ctrl Pts',(7.62776096538883,19.5264621687521,0.));
#16811=CARTESIAN_POINT('Ctrl Pts',(7.6232405373522,19.5769527121826,0.));
#16812=CARTESIAN_POINT('Ctrl Pts',(7.61844037070591,19.6274933688524,0.));
#16813=CARTESIAN_POINT('Ctrl Pts',(7.61336212350879,19.6780827744426,0.));
#16814=CARTESIAN_POINT('Ctrl Pts',(7.60800746969262,19.7287195480601,0.));
#16815=CARTESIAN_POINT('Ctrl Pts',(7.60237814110187,19.7794022782484,0.));
#16816=CARTESIAN_POINT('Ctrl Pts',(7.59647587605448,19.830129556152,0.));
#16817=CARTESIAN_POINT('Ctrl Pts',(7.59030238888852,19.8808999994024,0.));
#16818=CARTESIAN_POINT('Ctrl Pts',(7.58385933533352,19.931712276832,0.));
#16819=CARTESIAN_POINT('Ctrl Pts',(7.57714827622806,19.9825651387294,0.));
#16820=CARTESIAN_POINT('Ctrl Pts',(7.57017066105973,20.0334574248557,0.));
#16821=CARTESIAN_POINT('Ctrl Pts',(7.5629278654946,20.0843880130978,0.));
#16822=CARTESIAN_POINT('Ctrl Pts',(7.55542122125495,20.1353557774357,0.));
#16823=CARTESIAN_POINT('Ctrl Pts',(7.54765204869254,20.1863595454674,0.));
#16824=CARTESIAN_POINT('Ctrl Pts',(7.53962169534167,20.2373980474879,0.));
#16825=CARTESIAN_POINT('Ctrl Pts',(7.53133155804008,20.2884698940944,0.));
#16826=CARTESIAN_POINT('Ctrl Pts',(7.52278303006887,20.3395736743243,0.));
#16827=CARTESIAN_POINT('Ctrl Pts',(7.51397746081994,20.3907080367098,0.));
#16828=CARTESIAN_POINT('Ctrl Pts',(7.50491611266253,20.4418717748497,0.));
#16829=CARTESIAN_POINT('Ctrl Pts',(7.49560012018406,20.4930639156161,0.));
#16830=CARTESIAN_POINT('Ctrl Pts',(7.48411651832413,20.5545277683621,0.));
#16831=CARTESIAN_POINT('Ctrl Pts',(7.47423073598682,20.6057817877246,0.));
#16832=CARTESIAN_POINT('Ctrl Pts',(7.46612041736314,20.6468066077586,0.));
#16833=CARTESIAN_POINT('Ctrl Pts',(7.45992433946824,20.6775873630604,0.));
#16834=CARTESIAN_POINT('Ctrl Pts',(7.45574324794401,20.698113262342,0.));
#16835=CARTESIAN_POINT('Ctrl Pts',(7.45007618140239,17.2541372868972,13.));
#16836=CARTESIAN_POINT('Ctrl Pts',(7.45637364573816,17.2687220121489,13.));
#16837=CARTESIAN_POINT('Ctrl Pts',(7.46226667103919,17.2834550499008,13.));
#16838=CARTESIAN_POINT('Ctrl Pts',(7.46778231425445,17.2983267669067,13.));
#16839=CARTESIAN_POINT('Ctrl Pts',(7.47424706065699,17.3157575315993,13.));
#16840=CARTESIAN_POINT('Ctrl Pts',(7.48019417753821,17.3333785326113,13.));
#16841=CARTESIAN_POINT('Ctrl Pts',(7.48573450280811,17.3511502187375,13.));
#16842=CARTESIAN_POINT('Ctrl Pts',(7.49353000563121,17.3761558316968,13.));
#16843=CARTESIAN_POINT('Ctrl Pts',(7.50052692940225,17.4014574303076,13.));
#16844=CARTESIAN_POINT('Ctrl Pts',(7.50711117101491,17.4269165094415,13.));
#16845=CARTESIAN_POINT('Ctrl Pts',(7.5114907300879,17.4438508122163,13.));
#16846=CARTESIAN_POINT('Ctrl Pts',(7.51568961154289,17.4608540901313,13.));
#16847=CARTESIAN_POINT('Ctrl Pts',(7.5197927693323,17.477895354957,13.));
#16848=CARTESIAN_POINT('Ctrl Pts',(7.5241120155096,17.4958340796498,13.));
#16849=CARTESIAN_POINT('Ctrl Pts',(7.52832602172349,17.5138146001176,13.));
#16850=CARTESIAN_POINT('Ctrl Pts',(7.53247314101595,17.5318219263294,13.));
#16851=CARTESIAN_POINT('Ctrl Pts',(7.53707874400533,17.5518200478164,13.));
#16852=CARTESIAN_POINT('Ctrl Pts',(7.54160061545783,17.5718516505933,13.));
#16853=CARTESIAN_POINT('Ctrl Pts',(7.54602601378991,17.5919190740375,13.));
#16854=CARTESIAN_POINT('Ctrl Pts',(7.55269751656652,17.6221716888714,13.));
#16855=CARTESIAN_POINT('Ctrl Pts',(7.55914375118896,17.652507694639,13.));
#16856=CARTESIAN_POINT('Ctrl Pts',(7.56521559976847,17.6829731243237,13.));
#16857=CARTESIAN_POINT('Ctrl Pts',(7.5696266650164,17.7051055929427,13.));
#16858=CARTESIAN_POINT('Ctrl Pts',(7.57383703867086,17.7273074810788,13.));
#16859=CARTESIAN_POINT('Ctrl Pts',(7.57782678310958,17.7495842480019,13.));
#16860=CARTESIAN_POINT('Ctrl Pts',(7.58270390405198,17.7768156880499,13.));
#16861=CARTESIAN_POINT('Ctrl Pts',(7.58725254420758,17.8041586050609,13.));
#16862=CARTESIAN_POINT('Ctrl Pts',(7.5915173324576,17.8315958505033,13.));
#16863=CARTESIAN_POINT('Ctrl Pts',(7.59612401157631,17.8612326292236,13.));
#16864=CARTESIAN_POINT('Ctrl Pts',(7.60040516926094,17.8909775513386,13.));
#16865=CARTESIAN_POINT('Ctrl Pts',(7.60444696777939,17.9207992272241,13.));
#16866=CARTESIAN_POINT('Ctrl Pts',(7.60817833718686,17.9483304583261,13.));
#16867=CARTESIAN_POINT('Ctrl Pts',(7.61170808544563,17.9759263070109,13.));
#16868=CARTESIAN_POINT('Ctrl Pts',(7.61506270604984,18.0035762489985,13.));
#16869=CARTESIAN_POINT('Ctrl Pts',(7.61962013038162,18.0411401148582,13.));
#16870=CARTESIAN_POINT('Ctrl Pts',(7.62385245909446,18.0788044381321,13.));
#16871=CARTESIAN_POINT('Ctrl Pts',(7.62773031180607,18.116575681107,13.));
#16872=CARTESIAN_POINT('Ctrl Pts',(7.63147235591991,18.1530241148041,13.));
#16873=CARTESIAN_POINT('Ctrl Pts',(7.63487692331691,18.1895746221268,13.));
#16874=CARTESIAN_POINT('Ctrl Pts',(7.6379279464237,18.2262298441586,13.));
#16875=CARTESIAN_POINT('Ctrl Pts',(7.6420728467974,18.2760269902896,13.));
#16876=CARTESIAN_POINT('Ctrl Pts',(7.64556831472686,18.3260163400101,13.));
#16877=CARTESIAN_POINT('Ctrl Pts',(7.64849356609469,18.3761647741644,13.));
#16878=CARTESIAN_POINT('Ctrl Pts',(7.6510647984552,18.4202441576132,13.));
#16879=CARTESIAN_POINT('Ctrl Pts',(7.65320196597345,18.4644442731511,13.));
#16880=CARTESIAN_POINT('Ctrl Pts',(7.65493429570875,18.5087513218552,13.));
#16881=CARTESIAN_POINT('Ctrl Pts',(7.65748817031438,18.5740706685303,13.));
#16882=CARTESIAN_POINT('Ctrl Pts',(7.65915358769477,18.6396252901549,13.));
#16883=CARTESIAN_POINT('Ctrl Pts',(7.65993127489918,18.705403439409,13.));
#16884=CARTESIAN_POINT('Ctrl Pts',(7.66091272374058,18.7884161056964,13.));
#16885=CARTESIAN_POINT('Ctrl Pts',(7.66048522719276,18.8717830757028,13.));
#16886=CARTESIAN_POINT('Ctrl Pts',(7.6587598380681,18.9554457129728,13.));
#16887=CARTESIAN_POINT('Ctrl Pts',(7.65642266547611,19.0687732053082,13.));
#16888=CARTESIAN_POINT('Ctrl Pts',(7.65169843823839,19.1826450749753,13.));
#16889=CARTESIAN_POINT('Ctrl Pts',(7.64469887385525,19.296975739756,13.));
#16890=CARTESIAN_POINT('Ctrl Pts',(7.63845857891208,19.3989045213524,13.));
#16891=CARTESIAN_POINT('Ctrl Pts',(7.63041784746716,19.5011952230932,13.));
#16892=CARTESIAN_POINT('Ctrl Pts',(7.62065725315594,19.6037897795266,13.));
#16893=CARTESIAN_POINT('Ctrl Pts',(7.60682380699052,19.7491944780556,13.));
#16894=CARTESIAN_POINT('Ctrl Pts',(7.58953015253691,19.8952104276061,13.));
#16895=CARTESIAN_POINT('Ctrl Pts',(7.56895177486366,20.041695755794,13.));
#16896=CARTESIAN_POINT('Ctrl Pts',(7.55296697986665,20.155482079397,13.));
#16897=CARTESIAN_POINT('Ctrl Pts',(7.53499708083853,20.2695554917631,13.));
#16898=CARTESIAN_POINT('Ctrl Pts',(7.51511029115765,20.3838501742203,13.));
#16899=CARTESIAN_POINT('Ctrl Pts',(7.49790671588851,20.482723708062,13.));
#16900=CARTESIAN_POINT('Ctrl Pts',(7.47927116735874,20.5817593865392,13.));
#16901=CARTESIAN_POINT('Ctrl Pts',(7.45922688154243,20.6809436222924,13.));
#16902=CARTESIAN_POINT('Ctrl Pts',(7.45807037082203,20.6866663321457,13.));
#16903=CARTESIAN_POINT('Ctrl Pts',(7.45690915953565,20.6923895455068,13.));
#16904=CARTESIAN_POINT('Ctrl Pts',(7.45574324794401,20.698113262342,13.));
#16905=CARTESIAN_POINT('Ctrl Pts',(12.3627494547115,18.1978687191668,0.));
#16906=CARTESIAN_POINT('Ctrl Pts',(12.3627494547115,18.1978687191668,21.));
#16907=CARTESIAN_POINT('Ctrl Pts',(12.3532177620787,18.1935275957711,0.));
#16908=CARTESIAN_POINT('Ctrl Pts',(12.3532177620787,18.1935275957711,21.));
#16909=CARTESIAN_POINT('Ctrl Pts',(12.3341713636489,18.1848265584754,0.));
#16910=CARTESIAN_POINT('Ctrl Pts',(12.3341713636489,18.1848265584754,21.));
#16911=CARTESIAN_POINT('Ctrl Pts',(12.3056527265146,18.1717186310224,0.));
#16912=CARTESIAN_POINT('Ctrl Pts',(12.3056527265146,18.1717186310224,21.));
#16913=CARTESIAN_POINT('Ctrl Pts',(12.2677298318549,18.1541286139166,0.));
#16914=CARTESIAN_POINT('Ctrl Pts',(12.2677298318549,18.1541286139166,21.));
#16915=CARTESIAN_POINT('Ctrl Pts',(12.2204964278426,18.1319528884305,0.));
#16916=CARTESIAN_POINT('Ctrl Pts',(12.2204964278426,18.1319528884305,21.));
#16917=CARTESIAN_POINT('Ctrl Pts',(12.1734337668195,18.109588624154,0.));
#16918=CARTESIAN_POINT('Ctrl Pts',(12.1734337668195,18.109588624154,21.));
#16919=CARTESIAN_POINT('Ctrl Pts',(12.1265426519718,18.0870354350128,0.));
#16920=CARTESIAN_POINT('Ctrl Pts',(12.1265426519718,18.0870354350128,21.));
#16921=CARTESIAN_POINT('Ctrl Pts',(12.0798241915081,18.0642929289333,0.));
#16922=CARTESIAN_POINT('Ctrl Pts',(12.0798241915081,18.0642929289333,21.));
#16923=CARTESIAN_POINT('Ctrl Pts',(12.0332798395991,18.0413607600052,0.));
#16924=CARTESIAN_POINT('Ctrl Pts',(12.0332798395991,18.0413607600052,21.));
#16925=CARTESIAN_POINT('Ctrl Pts',(11.986911314246,18.0182386160553,0.));
#16926=CARTESIAN_POINT('Ctrl Pts',(11.986911314246,18.0182386160553,21.));
#16927=CARTESIAN_POINT('Ctrl Pts',(11.9407205019619,17.9949261997754,0.));
#16928=CARTESIAN_POINT('Ctrl Pts',(11.9407205019619,17.9949261997754,21.));
#16929=CARTESIAN_POINT('Ctrl Pts',(11.8947093631895,17.9714232133203,0.));
#16930=CARTESIAN_POINT('Ctrl Pts',(11.8947093631895,17.9714232133203,21.));
#16931=CARTESIAN_POINT('Ctrl Pts',(11.8488798430201,17.9477293432951,0.));
#16932=CARTESIAN_POINT('Ctrl Pts',(11.8488798430201,17.9477293432951,21.));
#16933=CARTESIAN_POINT('Ctrl Pts',(11.8032337607271,17.9238442458356,0.));
#16934=CARTESIAN_POINT('Ctrl Pts',(11.8032337607271,17.9238442458356,21.));
#16935=CARTESIAN_POINT('Ctrl Pts',(11.7577728408871,17.8997675418752,0.));
#16936=CARTESIAN_POINT('Ctrl Pts',(11.7577728408871,17.8997675418752,21.));
#16937=CARTESIAN_POINT('Ctrl Pts',(11.7124987772363,17.8754988158862,0.));
#16938=CARTESIAN_POINT('Ctrl Pts',(11.7124987772363,17.8754988158862,21.));
#16939=CARTESIAN_POINT('Ctrl Pts',(11.6674132861792,17.8510376144926,0.));
#16940=CARTESIAN_POINT('Ctrl Pts',(11.6674132861792,17.8510376144926,21.));
#16941=CARTESIAN_POINT('Ctrl Pts',(11.6225181583564,17.8263834470057,0.));
#16942=CARTESIAN_POINT('Ctrl Pts',(11.6225181583564,17.8263834470057,21.));
#16943=CARTESIAN_POINT('Ctrl Pts',(11.5778153222435,17.8015357852426,0.));
#16944=CARTESIAN_POINT('Ctrl Pts',(11.5778153222435,17.8015357852426,21.));
#16945=CARTESIAN_POINT('Ctrl Pts',(11.5333068279911,17.7764940721306,0.));
#16946=CARTESIAN_POINT('Ctrl Pts',(11.5333068279911,17.7764940721306,21.));
#16947=CARTESIAN_POINT('Ctrl Pts',(11.4889948016216,17.7512577332768,0.));
#16948=CARTESIAN_POINT('Ctrl Pts',(11.4889948016216,17.7512577332768,21.));
#16949=CARTESIAN_POINT('Ctrl Pts',(11.4448814046804,17.725826190457,0.));
#16950=CARTESIAN_POINT('Ctrl Pts',(11.4448814046804,17.725826190457,21.));
#16951=CARTESIAN_POINT('Ctrl Pts',(11.4009687970126,17.700198872213,0.));
#16952=CARTESIAN_POINT('Ctrl Pts',(11.4009687970126,17.700198872213,21.));
#16953=CARTESIAN_POINT('Ctrl Pts',(11.3572590796967,17.674375235974,0.));
#16954=CARTESIAN_POINT('Ctrl Pts',(11.3572590796967,17.674375235974,21.));
#16955=CARTESIAN_POINT('Ctrl Pts',(11.3137543310722,17.6483547422688,0.));
#16956=CARTESIAN_POINT('Ctrl Pts',(11.3137543310722,17.6483547422688,21.));
#16957=CARTESIAN_POINT('Ctrl Pts',(11.2704566868205,17.6221368072528,0.));
#16958=CARTESIAN_POINT('Ctrl Pts',(11.2704566868205,17.6221368072528,21.));
#16959=CARTESIAN_POINT('Ctrl Pts',(11.2273684103051,17.5957207597803,0.));
#16960=CARTESIAN_POINT('Ctrl Pts',(11.2273684103051,17.5957207597803,21.));
#16961=CARTESIAN_POINT('Ctrl Pts',(11.1844919535058,17.5691058058227,0.));
#16962=CARTESIAN_POINT('Ctrl Pts',(11.1844919535058,17.5691058058227,21.));
#16963=CARTESIAN_POINT('Ctrl Pts',(11.1418300507683,17.5422909714139,0.));
#16964=CARTESIAN_POINT('Ctrl Pts',(11.1418300507683,17.5422909714139,21.));
#16965=CARTESIAN_POINT('Ctrl Pts',(11.0993856581394,17.5152751467292,0.));
#16966=CARTESIAN_POINT('Ctrl Pts',(11.0993856581394,17.5152751467292,21.));
#16967=CARTESIAN_POINT('Ctrl Pts',(11.0571618040371,17.4880571878157,0.));
#16968=CARTESIAN_POINT('Ctrl Pts',(11.0571618040371,17.4880571878157,21.));
#16969=CARTESIAN_POINT('Ctrl Pts',(11.0151614525642,17.460636011184,0.));
#16970=CARTESIAN_POINT('Ctrl Pts',(11.0151614525642,17.460636011184,21.));
#16971=CARTESIAN_POINT('Ctrl Pts',(10.9733873885115,17.4330106728622,0.));
#16972=CARTESIAN_POINT('Ctrl Pts',(10.9733873885115,17.4330106728622,21.));
#16973=CARTESIAN_POINT('Ctrl Pts',(10.9318420203801,17.4051805054129,0.));
#16974=CARTESIAN_POINT('Ctrl Pts',(10.9318420203801,17.4051805054129,21.));
#16975=CARTESIAN_POINT('Ctrl Pts',(10.8905275295837,17.377145012528,0.));
#16976=CARTESIAN_POINT('Ctrl Pts',(10.8905275295837,17.377145012528,21.));
#16977=CARTESIAN_POINT('Ctrl Pts',(10.8494462423128,17.3489036079991,0.));
#16978=CARTESIAN_POINT('Ctrl Pts',(10.8494462423128,17.3489036079991,21.));
#16979=CARTESIAN_POINT('Ctrl Pts',(10.8086009632423,17.3204553814537,0.));
#16980=CARTESIAN_POINT('Ctrl Pts',(10.8086009632423,17.3204553814537,21.));
#16981=CARTESIAN_POINT('Ctrl Pts',(10.7679952591482,17.2917988998581,0.));
#16982=CARTESIAN_POINT('Ctrl Pts',(10.7679952591482,17.2917988998581,21.));
#16983=CARTESIAN_POINT('Ctrl Pts',(10.7276339231608,17.2629318816279,0.));
#16984=CARTESIAN_POINT('Ctrl Pts',(10.7276339231608,17.2629318816279,21.));
#16985=CARTESIAN_POINT('Ctrl Pts',(10.6875226650217,17.2338514174708,0.));
#16986=CARTESIAN_POINT('Ctrl Pts',(10.6875226650217,17.2338514174708,21.));
#16987=CARTESIAN_POINT('Ctrl Pts',(10.6476672831754,17.2045545572011,0.));
#16988=CARTESIAN_POINT('Ctrl Pts',(10.6476672831754,17.2045545572011,21.));
#16989=CARTESIAN_POINT('Ctrl Pts',(10.6080729180997,17.1750388395657,0.));
#16990=CARTESIAN_POINT('Ctrl Pts',(10.6080729180997,17.1750388395657,21.));
#16991=CARTESIAN_POINT('Ctrl Pts',(10.5687434234512,17.1453027387554,0.));
#16992=CARTESIAN_POINT('Ctrl Pts',(10.5687434234512,17.1453027387554,21.));
#16993=CARTESIAN_POINT('Ctrl Pts',(10.5296803023445,17.1153464189932,0.));
#16994=CARTESIAN_POINT('Ctrl Pts',(10.5296803023445,17.1153464189932,21.));
#16995=CARTESIAN_POINT('Ctrl Pts',(10.4908835057575,17.0851711712016,0.));
#16996=CARTESIAN_POINT('Ctrl Pts',(10.4908835057575,17.0851711712016,21.));
#16997=CARTESIAN_POINT('Ctrl Pts',(10.452353435089,17.0547779975888,0.));
#16998=CARTESIAN_POINT('Ctrl Pts',(10.452353435089,17.0547779975888,21.));
#16999=CARTESIAN_POINT('Ctrl Pts',(10.4140927470882,17.0241663361802,0.));
#17000=CARTESIAN_POINT('Ctrl Pts',(10.4140927470882,17.0241663361802,21.));
#17001=CARTESIAN_POINT('Ctrl Pts',(10.3761078860454,16.9933329788855,0.));
#17002=CARTESIAN_POINT('Ctrl Pts',(10.3761078860454,16.9933329788855,21.));
#17003=CARTESIAN_POINT('Ctrl Pts',(10.3384116178624,16.9622702798438,0.));
#17004=CARTESIAN_POINT('Ctrl Pts',(10.3384116178624,16.9622702798438,21.));
#17005=CARTESIAN_POINT('Ctrl Pts',(10.3010210756062,16.9309675442426,0.));
#17006=CARTESIAN_POINT('Ctrl Pts',(10.3010210756062,16.9309675442426,21.));
#17007=CARTESIAN_POINT('Ctrl Pts',(10.2639532144219,16.8994142530447,0.));
#17008=CARTESIAN_POINT('Ctrl Pts',(10.2639532144219,16.8994142530447,21.));
#17009=CARTESIAN_POINT('Ctrl Pts',(10.2272206796636,16.8676029947679,0.));
#17010=CARTESIAN_POINT('Ctrl Pts',(10.2272206796636,16.8676029947679,21.));
#17011=CARTESIAN_POINT('Ctrl Pts',(10.1908283166713,16.8355319435838,0.));
#17012=CARTESIAN_POINT('Ctrl Pts',(10.1908283166713,16.8355319435838,21.));
#17013=CARTESIAN_POINT('Ctrl Pts',(10.1547673397274,16.8032089941901,0.));
#17014=CARTESIAN_POINT('Ctrl Pts',(10.1547673397274,16.8032089941901,21.));
#17015=CARTESIAN_POINT('Ctrl Pts',(10.1190207721353,16.7706479198888,0.));
#17016=CARTESIAN_POINT('Ctrl Pts',(10.1190207721353,16.7706479198888,21.));
#17017=CARTESIAN_POINT('Ctrl Pts',(10.0835742491038,16.7378607357337,0.));
#17018=CARTESIAN_POINT('Ctrl Pts',(10.0835742491038,16.7378607357337,21.));
#17019=CARTESIAN_POINT('Ctrl Pts',(10.0484259314257,16.7048506904207,0.));
#17020=CARTESIAN_POINT('Ctrl Pts',(10.0484259314257,16.7048506904207,21.));
#17021=CARTESIAN_POINT('Ctrl Pts',(10.0135950379525,16.6716062376277,0.));
#17022=CARTESIAN_POINT('Ctrl Pts',(10.0135950379525,16.6716062376277,21.));
#17023=CARTESIAN_POINT('Ctrl Pts',(9.97913546489641,16.6380914029057,0.));
#17024=CARTESIAN_POINT('Ctrl Pts',(9.97913546489641,16.6380914029057,21.));
#17025=CARTESIAN_POINT('Ctrl Pts',(9.9451214271291,16.6042559779574,0.));
#17026=CARTESIAN_POINT('Ctrl Pts',(9.9451214271291,16.6042559779574,21.));
#17027=CARTESIAN_POINT('Ctrl Pts',(9.91162317616649,16.5700527532381,0.));
#17028=CARTESIAN_POINT('Ctrl Pts',(9.91162317616649,16.5700527532381,21.));
#17029=CARTESIAN_POINT('Ctrl Pts',(9.8786843754698,16.5354535643506,0.));
#17030=CARTESIAN_POINT('Ctrl Pts',(9.8786843754698,16.5354535643506,21.));
#17031=CARTESIAN_POINT('Ctrl Pts',(9.84630229363521,16.5004633692332,0.));
#17032=CARTESIAN_POINT('Ctrl Pts',(9.84630229363521,16.5004633692332,21.));
#17033=CARTESIAN_POINT('Ctrl Pts',(9.81439757053278,16.4651416449558,0.));
#17034=CARTESIAN_POINT('Ctrl Pts',(9.81439757053278,16.4651416449558,21.));
#17035=CARTESIAN_POINT('Ctrl Pts',(9.78285689698057,16.4295725710378,0.));
#17036=CARTESIAN_POINT('Ctrl Pts',(9.78285689698057,16.4295725710378,21.));
#17037=CARTESIAN_POINT('Ctrl Pts',(9.75159288382684,16.3938231282759,0.));
#17038=CARTESIAN_POINT('Ctrl Pts',(9.75159288382684,16.3938231282759,21.));
#17039=CARTESIAN_POINT('Ctrl Pts',(9.72060002001011,16.3579039682519,0.));
#17040=CARTESIAN_POINT('Ctrl Pts',(9.72060002001011,16.3579039682519,21.));
#17041=CARTESIAN_POINT('Ctrl Pts',(9.69000797146315,16.3217321000366,0.));
#17042=CARTESIAN_POINT('Ctrl Pts',(9.69000797146315,16.3217321000366,21.));
#17043=CARTESIAN_POINT('Ctrl Pts',(9.66014786078746,16.2850845948324,0.));
#17044=CARTESIAN_POINT('Ctrl Pts',(9.66014786078746,16.2850845948324,21.));
#17045=CARTESIAN_POINT('Ctrl Pts',(9.63146315443273,16.2476599387841,0.));
#17046=CARTESIAN_POINT('Ctrl Pts',(9.63146315443273,16.2476599387841,21.));
#17047=CARTESIAN_POINT('Ctrl Pts',(9.60981421781524,16.2168537871666,0.));
#17048=CARTESIAN_POINT('Ctrl Pts',(9.60981421781524,16.2168537871666,21.));
#17049=CARTESIAN_POINT('Ctrl Pts',(9.59446643316596,16.1931534965272,0.));
#17050=CARTESIAN_POINT('Ctrl Pts',(9.59446643316596,16.1931534965272,21.));
#17051=CARTESIAN_POINT('Ctrl Pts',(9.58464985151482,16.1770747160769,0.));
#17052=CARTESIAN_POINT('Ctrl Pts',(9.58464985151482,16.1770747160769,21.));
#17053=CARTESIAN_POINT('Ctrl Pts',(9.57984538049455,16.1689656784104,0.));
#17054=CARTESIAN_POINT('Ctrl Pts',(9.57984538049455,16.1689656784104,21.));
#17055=CARTESIAN_POINT('',(12.3627494547114,18.1978687191669,0.));
#17056=CARTESIAN_POINT('Ctrl Pts',(9.57984538049455,16.1689656784104,0.));
#17057=CARTESIAN_POINT('Ctrl Pts',(9.58464985151482,16.1770747160769,0.));
#17058=CARTESIAN_POINT('Ctrl Pts',(9.59446643316596,16.1931534965272,0.));
#17059=CARTESIAN_POINT('Ctrl Pts',(9.60981421781524,16.2168537871666,0.));
#17060=CARTESIAN_POINT('Ctrl Pts',(9.63146315443273,16.2476599387841,0.));
#17061=CARTESIAN_POINT('Ctrl Pts',(9.66014786078746,16.2850845948324,0.));
#17062=CARTESIAN_POINT('Ctrl Pts',(9.69000797146315,16.3217321000366,0.));
#17063=CARTESIAN_POINT('Ctrl Pts',(9.72060002001011,16.3579039682519,0.));
#17064=CARTESIAN_POINT('Ctrl Pts',(9.75159288382684,16.3938231282759,0.));
#17065=CARTESIAN_POINT('Ctrl Pts',(9.78285689698057,16.4295725710378,0.));
#17066=CARTESIAN_POINT('Ctrl Pts',(9.81439757053278,16.4651416449558,0.));
#17067=CARTESIAN_POINT('Ctrl Pts',(9.84630229363521,16.5004633692332,0.));
#17068=CARTESIAN_POINT('Ctrl Pts',(9.8786843754698,16.5354535643506,0.));
#17069=CARTESIAN_POINT('Ctrl Pts',(9.91162317616649,16.5700527532381,0.));
#17070=CARTESIAN_POINT('Ctrl Pts',(9.9451214271291,16.6042559779574,0.));
#17071=CARTESIAN_POINT('Ctrl Pts',(9.97913546489641,16.6380914029057,0.));
#17072=CARTESIAN_POINT('Ctrl Pts',(10.0135950379525,16.6716062376277,0.));
#17073=CARTESIAN_POINT('Ctrl Pts',(10.0484259314257,16.7048506904207,0.));
#17074=CARTESIAN_POINT('Ctrl Pts',(10.0835742491038,16.7378607357337,0.));
#17075=CARTESIAN_POINT('Ctrl Pts',(10.1190207721353,16.7706479198888,0.));
#17076=CARTESIAN_POINT('Ctrl Pts',(10.1547673397274,16.8032089941901,0.));
#17077=CARTESIAN_POINT('Ctrl Pts',(10.1908283166713,16.8355319435838,0.));
#17078=CARTESIAN_POINT('Ctrl Pts',(10.2272206796636,16.8676029947679,0.));
#17079=CARTESIAN_POINT('Ctrl Pts',(10.2639532144219,16.8994142530447,0.));
#17080=CARTESIAN_POINT('Ctrl Pts',(10.3010210756062,16.9309675442426,0.));
#17081=CARTESIAN_POINT('Ctrl Pts',(10.3384116178624,16.9622702798438,0.));
#17082=CARTESIAN_POINT('Ctrl Pts',(10.3761078860454,16.9933329788855,0.));
#17083=CARTESIAN_POINT('Ctrl Pts',(10.4140927470882,17.0241663361802,0.));
#17084=CARTESIAN_POINT('Ctrl Pts',(10.452353435089,17.0547779975888,0.));
#17085=CARTESIAN_POINT('Ctrl Pts',(10.4908835057575,17.0851711712016,0.));
#17086=CARTESIAN_POINT('Ctrl Pts',(10.5296803023445,17.1153464189932,0.));
#17087=CARTESIAN_POINT('Ctrl Pts',(10.5687434234512,17.1453027387554,0.));
#17088=CARTESIAN_POINT('Ctrl Pts',(10.6080729180997,17.1750388395657,0.));
#17089=CARTESIAN_POINT('Ctrl Pts',(10.6476672831754,17.2045545572011,0.));
#17090=CARTESIAN_POINT('Ctrl Pts',(10.6875226650217,17.2338514174708,0.));
#17091=CARTESIAN_POINT('Ctrl Pts',(10.7276339231608,17.2629318816279,0.));
#17092=CARTESIAN_POINT('Ctrl Pts',(10.7679952591482,17.2917988998581,0.));
#17093=CARTESIAN_POINT('Ctrl Pts',(10.8086009632423,17.3204553814537,0.));
#17094=CARTESIAN_POINT('Ctrl Pts',(10.8494462423128,17.3489036079991,0.));
#17095=CARTESIAN_POINT('Ctrl Pts',(10.8905275295837,17.377145012528,0.));
#17096=CARTESIAN_POINT('Ctrl Pts',(10.9318420203801,17.4051805054129,0.));
#17097=CARTESIAN_POINT('Ctrl Pts',(10.9733873885115,17.4330106728622,0.));
#17098=CARTESIAN_POINT('Ctrl Pts',(11.0151614525642,17.460636011184,0.));
#17099=CARTESIAN_POINT('Ctrl Pts',(11.0571618040371,17.4880571878157,0.));
#17100=CARTESIAN_POINT('Ctrl Pts',(11.0993856581394,17.5152751467292,0.));
#17101=CARTESIAN_POINT('Ctrl Pts',(11.1418300507683,17.5422909714139,0.));
#17102=CARTESIAN_POINT('Ctrl Pts',(11.1844919535058,17.5691058058227,0.));
#17103=CARTESIAN_POINT('Ctrl Pts',(11.2273684103051,17.5957207597803,0.));
#17104=CARTESIAN_POINT('Ctrl Pts',(11.2704566868205,17.6221368072528,0.));
#17105=CARTESIAN_POINT('Ctrl Pts',(11.3137543310722,17.6483547422688,0.));
#17106=CARTESIAN_POINT('Ctrl Pts',(11.3572590796967,17.674375235974,0.));
#17107=CARTESIAN_POINT('Ctrl Pts',(11.4009687970126,17.700198872213,0.));
#17108=CARTESIAN_POINT('Ctrl Pts',(11.4448814046804,17.725826190457,0.));
#17109=CARTESIAN_POINT('Ctrl Pts',(11.4889948016216,17.7512577332768,0.));
#17110=CARTESIAN_POINT('Ctrl Pts',(11.5333068279911,17.7764940721306,0.));
#17111=CARTESIAN_POINT('Ctrl Pts',(11.5778153222435,17.8015357852426,0.));
#17112=CARTESIAN_POINT('Ctrl Pts',(11.6225181583564,17.8263834470057,0.));
#17113=CARTESIAN_POINT('Ctrl Pts',(11.6674132861792,17.8510376144926,0.));
#17114=CARTESIAN_POINT('Ctrl Pts',(11.7124987772363,17.8754988158862,0.));
#17115=CARTESIAN_POINT('Ctrl Pts',(11.7577728408871,17.8997675418752,0.));
#17116=CARTESIAN_POINT('Ctrl Pts',(11.8032337607271,17.9238442458356,0.));
#17117=CARTESIAN_POINT('Ctrl Pts',(11.8488798430201,17.9477293432951,0.));
#17118=CARTESIAN_POINT('Ctrl Pts',(11.8947093631895,17.9714232133203,0.));
#17119=CARTESIAN_POINT('Ctrl Pts',(11.9407205019619,17.9949261997754,0.));
#17120=CARTESIAN_POINT('Ctrl Pts',(11.986911314246,18.0182386160553,0.));
#17121=CARTESIAN_POINT('Ctrl Pts',(12.0332798395991,18.0413607600052,0.));
#17122=CARTESIAN_POINT('Ctrl Pts',(12.0798241915081,18.0642929289333,0.));
#17123=CARTESIAN_POINT('Ctrl Pts',(12.1265426519718,18.0870354350128,0.));
#17124=CARTESIAN_POINT('Ctrl Pts',(12.1734337668195,18.109588624154,0.));
#17125=CARTESIAN_POINT('Ctrl Pts',(12.2299089600472,18.1364257412858,0.));
#17126=CARTESIAN_POINT('Ctrl Pts',(12.2771850498068,18.1585543320743,0.));
#17127=CARTESIAN_POINT('Ctrl Pts',(12.3151419520839,18.1761067306718,0.));
#17128=CARTESIAN_POINT('Ctrl Pts',(12.3436860694314,18.1891864723772,0.));
#17129=CARTESIAN_POINT('Ctrl Pts',(12.3627494547115,18.1978687191668,0.));
#17130=CARTESIAN_POINT('',(12.3627494547114,18.1978687191669,13.));
#17131=CARTESIAN_POINT('Ctrl Pts',(12.3627494547115,18.1978687191668,13.));
#17132=CARTESIAN_POINT('Ctrl Pts',(12.2657596014803,18.1536955657482,13.));
#17133=CARTESIAN_POINT('Ctrl Pts',(12.169023050136,18.1079923296861,13.));
#17134=CARTESIAN_POINT('Ctrl Pts',(12.0727475247274,18.0607552358515,13.));
#17135=CARTESIAN_POINT('Ctrl Pts',(11.9463830806602,17.9987551680626,13.));
#17136=CARTESIAN_POINT('Ctrl Pts',(11.8208236442934,17.9341116361939,13.));
#17137=CARTESIAN_POINT('Ctrl Pts',(11.6966194524201,17.8668433674001,13.));
#17138=CARTESIAN_POINT('Ctrl Pts',(11.5669851023492,17.7966341564713,13.));
#17139=CARTESIAN_POINT('Ctrl Pts',(11.4388217697851,17.7235639107164,13.));
#17140=CARTESIAN_POINT('Ctrl Pts',(11.3127555917358,17.6476730730182,13.));
#17141=CARTESIAN_POINT('Ctrl Pts',(11.1945685498145,17.5765254126762,13.));
#17142=CARTESIAN_POINT('Ctrl Pts',(11.0782188859152,17.5029025452135,13.));
#17143=CARTESIAN_POINT('Ctrl Pts',(10.9642554050871,17.4268346378942,13.));
#17144=CARTESIAN_POINT('Ctrl Pts',(10.9600254617552,17.4240112515339,13.));
#17145=CARTESIAN_POINT('Ctrl Pts',(10.9557986898388,17.4211844233848,13.));
#17146=CARTESIAN_POINT('Ctrl Pts',(10.9515873193929,17.4183623684055,13.));
#17147=CARTESIAN_POINT('Ctrl Pts',(10.8848661681826,17.3736522771363,13.));
#17148=CARTESIAN_POINT('Ctrl Pts',(10.821246862648,17.3296352982567,13.));
#17149=CARTESIAN_POINT('Ctrl Pts',(10.7606710931032,17.2864928503383,13.));
#17150=CARTESIAN_POINT('Ctrl Pts',(10.7071165337234,17.2483509529062,13.));
#17151=CARTESIAN_POINT('Ctrl Pts',(10.6559465493499,17.2108884656131,13.));
#17152=CARTESIAN_POINT('Ctrl Pts',(10.6071256521871,17.1742227594056,13.));
#17153=CARTESIAN_POINT('Ctrl Pts',(10.5586309624272,17.1378020430589,13.));
#17154=CARTESIAN_POINT('Ctrl Pts',(10.5124511278601,17.1021695681408,13.));
#17155=CARTESIAN_POINT('Ctrl Pts',(10.4685087734972,17.0674664166947,13.));
#17156=CARTESIAN_POINT('Ctrl Pts',(10.4297467459301,17.0368543902677,13.));
#17157=CARTESIAN_POINT('Ctrl Pts',(10.3927227952995,17.0069675134053,13.));
#17158=CARTESIAN_POINT('Ctrl Pts',(10.3574204589883,16.9778741242538,13.));
#17159=CARTESIAN_POINT('Ctrl Pts',(10.3251177699006,16.9512528067301,13.));
#17160=CARTESIAN_POINT('Ctrl Pts',(10.294261944748,16.9252920099693,13.));
#17161=CARTESIAN_POINT('Ctrl Pts',(10.2648422441037,16.900041094165,13.));
#17162=CARTESIAN_POINT('Ctrl Pts',(10.2348002062189,16.8742560265875,13.));
#17163=CARTESIAN_POINT('Ctrl Pts',(10.2062569586814,16.849210296515,13.));
#17164=CARTESIAN_POINT('Ctrl Pts',(10.1791517798772,16.8249897307869,13.));
#17165=CARTESIAN_POINT('Ctrl Pts',(10.1529843049216,16.8016070756981,13.));
#17166=CARTESIAN_POINT('Ctrl Pts',(10.1281515192515,16.778997431011,13.));
#17167=CARTESIAN_POINT('Ctrl Pts',(10.104594858302,16.7572394204805,13.));
#17168=CARTESIAN_POINT('Ctrl Pts',(10.0816981615767,16.736090983122,13.));
#17169=CARTESIAN_POINT('Ctrl Pts',(10.0600064453471,16.7157475741055,13.));
#17170=CARTESIAN_POINT('Ctrl Pts',(10.0395060154369,16.6962518487154,13.));
#17171=CARTESIAN_POINT('Ctrl Pts',(10.0146112621281,16.6725771610972,13.));
#17172=CARTESIAN_POINT('Ctrl Pts',(9.99147913670146,16.6501483869943,13.));
#17173=CARTESIAN_POINT('Ctrl Pts',(9.97012646745884,16.6290105279122,13.));
#17174=CARTESIAN_POINT('Ctrl Pts',(9.95071237566143,16.6097917439767,13.));
#17175=CARTESIAN_POINT('Ctrl Pts',(9.93277105321012,16.5916388348028,13.));
#17176=CARTESIAN_POINT('Ctrl Pts',(9.91627156066964,16.5746150219053,13.));
#17177=CARTESIAN_POINT('Ctrl Pts',(9.89217566126396,16.5497534037634,13.));
#17178=CARTESIAN_POINT('Ctrl Pts',(9.87115249083465,16.5273017471855,13.));
#17179=CARTESIAN_POINT('Ctrl Pts',(9.85298457624544,16.5075382670064,13.));
#17180=CARTESIAN_POINT('Ctrl Pts',(9.8397201346617,16.4931088988453,13.));
#17181=CARTESIAN_POINT('Ctrl Pts',(9.82797372144175,16.4801151434696,13.));
#17182=CARTESIAN_POINT('Ctrl Pts',(9.81768546292149,16.4686464995442,13.));
#17183=CARTESIAN_POINT('Ctrl Pts',(9.81140156894346,16.4616416461614,13.));
#17184=CARTESIAN_POINT('Ctrl Pts',(9.80566257035652,16.4552050742887,13.));
#17185=CARTESIAN_POINT('Ctrl Pts',(9.80046232294511,16.4493517473189,13.));
#17186=CARTESIAN_POINT('Ctrl Pts',(9.79879887487039,16.4474793930427,13.));
#17187=CARTESIAN_POINT('Ctrl Pts',(9.79719059001671,16.4456666910777,13.));
#17188=CARTESIAN_POINT('Ctrl Pts',(9.79563736221273,16.4439140626976,13.));
#17189=CARTESIAN_POINT('Ctrl Pts',(9.79500566407819,16.4432012682991,13.));
#17190=CARTESIAN_POINT('Ctrl Pts',(9.79438446351028,16.4424999805057,13.));
#17191=CARTESIAN_POINT('Ctrl Pts',(9.79376929391731,16.4418051873884,13.));
#17192=CARTESIAN_POINT('Ctrl Pts',(9.77984315351516,16.4260765385531,13.));
#17193=CARTESIAN_POINT('Ctrl Pts',(9.76683512585064,16.4112295751864,13.));
#17194=CARTESIAN_POINT('Ctrl Pts',(9.75465239268516,16.3972210812639,13.));
#17195=CARTESIAN_POINT('Ctrl Pts',(9.73997218062171,16.3803408247009,13.));
#17196=CARTESIAN_POINT('Ctrl Pts',(9.72649172856169,16.3646770770088,13.));
#17197=CARTESIAN_POINT('Ctrl Pts',(9.71411692998175,16.3501049923794,13.));
#17198=CARTESIAN_POINT('Ctrl Pts',(9.70072429268956,16.334334340213,13.));
#17199=CARTESIAN_POINT('Ctrl Pts',(9.68863308112708,16.3198378092419,13.));
#17200=CARTESIAN_POINT('Ctrl Pts',(9.67773230410014,16.3064499392455,13.));
#17201=CARTESIAN_POINT('Ctrl Pts',(9.66640622721792,16.2925397340835,13.));
#17202=CARTESIAN_POINT('Ctrl Pts',(9.65636576393748,16.279825988344,13.));
#17203=CARTESIAN_POINT('Ctrl Pts',(9.64743434299806,16.2681588091213,13.));
#17204=CARTESIAN_POINT('Ctrl Pts',(9.63114001841937,16.2468734160732,13.));
#17205=CARTESIAN_POINT('Ctrl Pts',(9.61852759006646,16.2290773159714,13.));
#17206=CARTESIAN_POINT('Ctrl Pts',(9.60835104757439,16.2139851574147,13.));
#17207=CARTESIAN_POINT('Ctrl Pts',(9.60185659561648,16.2043536643252,13.));
#17208=CARTESIAN_POINT('Ctrl Pts',(9.59635317286195,16.1958243014909,13.));
#17209=CARTESIAN_POINT('Ctrl Pts',(9.59155330605552,16.1881695092273,13.));
#17210=CARTESIAN_POINT('Ctrl Pts',(9.58711261470323,16.1810875273349,13.));
#17211=CARTESIAN_POINT('Ctrl Pts',(9.58327471391801,16.1747537441068,13.));
#17212=CARTESIAN_POINT('Ctrl Pts',(9.57984538049455,16.1689656784104,13.));
#17213=CARTESIAN_POINT('',(12.3627494547114,18.1978687191669,0.));
#17214=CARTESIAN_POINT('Origin',(3.33073116609659E-12,4.58435815896522E-12,
0.));
#17215=CARTESIAN_POINT('',(13.4869019493419,17.3811241238545,0.));
#17216=CARTESIAN_POINT('Origin',(3.33073116609659E-12,4.58435815896522E-12,
0.));
#17217=CARTESIAN_POINT('',(13.4869019493419,17.3811241238545,13.));
#17218=CARTESIAN_POINT('Origin',(3.33073116609659E-12,4.58435815896522E-12,
13.));
#17219=CARTESIAN_POINT('',(13.4869019493419,17.3811241238545,0.));
#17220=CARTESIAN_POINT('Ctrl Pts',(12.4172651441477,14.1074595503134,0.));
#17221=CARTESIAN_POINT('Ctrl Pts',(12.4172651441477,14.1074595503134,21.));
#17222=CARTESIAN_POINT('Ctrl Pts',(12.4234926340671,14.1145347042316,0.));
#17223=CARTESIAN_POINT('Ctrl Pts',(12.4234926340671,14.1145347042316,21.));
#17224=CARTESIAN_POINT('Ctrl Pts',(12.4357509724316,14.1288394445866,0.));
#17225=CARTESIAN_POINT('Ctrl Pts',(12.4357509724316,14.1288394445866,21.));
#17226=CARTESIAN_POINT('Ctrl Pts',(12.4535485619996,14.1507598477672,0.));
#17227=CARTESIAN_POINT('Ctrl Pts',(12.4535485619996,14.1507598477672,21.));
#17228=CARTESIAN_POINT('Ctrl Pts',(12.4761570639125,14.1808688343892,0.));
#17229=CARTESIAN_POINT('Ctrl Pts',(12.4761570639125,14.1808688343892,21.));
#17230=CARTESIAN_POINT('Ctrl Pts',(12.5028859651751,14.2197144660135,0.));
#17231=CARTESIAN_POINT('Ctrl Pts',(12.5028859651751,14.2197144660135,21.));
#17232=CARTESIAN_POINT('Ctrl Pts',(12.5285125321527,14.2594378207584,0.));
#17233=CARTESIAN_POINT('Ctrl Pts',(12.5285125321527,14.2594378207584,21.));
#17234=CARTESIAN_POINT('Ctrl Pts',(12.5534605602317,14.2997103098726,0.));
#17235=CARTESIAN_POINT('Ctrl Pts',(12.5534605602317,14.2997103098726,21.));
#17236=CARTESIAN_POINT('Ctrl Pts',(12.5780443898087,14.3402859058353,0.));
#17237=CARTESIAN_POINT('Ctrl Pts',(12.5780443898087,14.3402859058353,21.));
#17238=CARTESIAN_POINT('Ctrl Pts',(12.6023830189244,14.3810669346235,0.));
#17239=CARTESIAN_POINT('Ctrl Pts',(12.6023830189244,14.3810669346235,21.));
#17240=CARTESIAN_POINT('Ctrl Pts',(12.626464614311,14.4220553460485,0.));
#17241=CARTESIAN_POINT('Ctrl Pts',(12.626464614311,14.4220553460485,21.));
#17242=CARTESIAN_POINT('Ctrl Pts',(12.6501984687124,14.463313553928,0.));
#17243=CARTESIAN_POINT('Ctrl Pts',(12.6501984687124,14.463313553928,21.));
#17244=CARTESIAN_POINT('Ctrl Pts',(12.6734695081852,14.5049233087958,0.));
#17245=CARTESIAN_POINT('Ctrl Pts',(12.6734695081852,14.5049233087958,21.));
#17246=CARTESIAN_POINT('Ctrl Pts',(12.6961966430455,14.5469417071951,0.));
#17247=CARTESIAN_POINT('Ctrl Pts',(12.6961966430455,14.5469417071951,21.));
#17248=CARTESIAN_POINT('Ctrl Pts',(12.7183743139638,14.5893698147583,0.));
#17249=CARTESIAN_POINT('Ctrl Pts',(12.7183743139638,14.5893698147583,21.));
#17250=CARTESIAN_POINT('Ctrl Pts',(12.7400427996251,14.6321748083434,0.));
#17251=CARTESIAN_POINT('Ctrl Pts',(12.7400427996251,14.6321748083434,21.));
#17252=CARTESIAN_POINT('Ctrl Pts',(12.7612687078867,14.6753044633399,0.));
#17253=CARTESIAN_POINT('Ctrl Pts',(12.7612687078867,14.6753044633399,21.));
#17254=CARTESIAN_POINT('Ctrl Pts',(12.7821227233337,14.7187037124277,0.));
#17255=CARTESIAN_POINT('Ctrl Pts',(12.7821227233337,14.7187037124277,21.));
#17256=CARTESIAN_POINT('Ctrl Pts',(12.8026557145457,14.7623324139791,0.));
#17257=CARTESIAN_POINT('Ctrl Pts',(12.8026557145457,14.7623324139791,21.));
#17258=CARTESIAN_POINT('Ctrl Pts',(12.8228846016791,14.8061758577898,0.));
#17259=CARTESIAN_POINT('Ctrl Pts',(12.8228846016791,14.8061758577898,21.));
#17260=CARTESIAN_POINT('Ctrl Pts',(12.8428057266944,14.8502347891476,0.));
#17261=CARTESIAN_POINT('Ctrl Pts',(12.8428057266944,14.8502347891476,21.));
#17262=CARTESIAN_POINT('Ctrl Pts',(12.8624032236317,14.8945191569251,0.));
#17263=CARTESIAN_POINT('Ctrl Pts',(12.8624032236317,14.8945191569251,21.));
#17264=CARTESIAN_POINT('Ctrl Pts',(12.8816587472147,14.9390408507356,0.));
#17265=CARTESIAN_POINT('Ctrl Pts',(12.8816587472147,14.9390408507356,21.));
#17266=CARTESIAN_POINT('Ctrl Pts',(12.9005620742036,14.9838057866976,0.));
#17267=CARTESIAN_POINT('Ctrl Pts',(12.9005620742036,14.9838057866976,21.));
#17268=CARTESIAN_POINT('Ctrl Pts',(12.9191164383568,15.0288099208306,0.));
#17269=CARTESIAN_POINT('Ctrl Pts',(12.9191164383568,15.0288099208306,21.));
#17270=CARTESIAN_POINT('Ctrl Pts',(12.9373327960422,15.0740435169624,0.));
#17271=CARTESIAN_POINT('Ctrl Pts',(12.9373327960422,15.0740435169624,21.));
#17272=CARTESIAN_POINT('Ctrl Pts',(12.9552263908864,15.1194937003528,0.));
#17273=CARTESIAN_POINT('Ctrl Pts',(12.9552263908864,15.1194937003528,21.));
#17274=CARTESIAN_POINT('Ctrl Pts',(12.9728126886697,15.1651474813659,0.));
#17275=CARTESIAN_POINT('Ctrl Pts',(12.9728126886697,15.1651474813659,21.));
#17276=CARTESIAN_POINT('Ctrl Pts',(12.9901029059182,15.2109950816083,0.));
#17277=CARTESIAN_POINT('Ctrl Pts',(12.9901029059182,15.2109950816083,21.));
#17278=CARTESIAN_POINT('Ctrl Pts',(13.0071020851025,15.2570313635503,0.));
#17279=CARTESIAN_POINT('Ctrl Pts',(13.0071020851025,15.2570313635503,21.));
#17280=CARTESIAN_POINT('Ctrl Pts',(13.0238115816728,15.3032539741328,0.));
#17281=CARTESIAN_POINT('Ctrl Pts',(13.0238115816728,15.3032539741328,21.));
#17282=CARTESIAN_POINT('Ctrl Pts',(13.0402305665115,15.3496622219036,0.));
#17283=CARTESIAN_POINT('Ctrl Pts',(13.0402305665115,15.3496622219036,21.));
#17284=CARTESIAN_POINT('Ctrl Pts',(13.0563577967298,15.3962557545684,0.));
#17285=CARTESIAN_POINT('Ctrl Pts',(13.0563577967298,15.3962557545684,21.));
#17286=CARTESIAN_POINT('Ctrl Pts',(13.0721935806302,15.4430330918328,0.));
#17287=CARTESIAN_POINT('Ctrl Pts',(13.0721935806302,15.4430330918328,21.));
#17288=CARTESIAN_POINT('Ctrl Pts',(13.087740560189,15.4899910401523,0.));
#17289=CARTESIAN_POINT('Ctrl Pts',(13.087740560189,15.4899910401523,21.));
#17290=CARTESIAN_POINT('Ctrl Pts',(13.1030026646917,15.5371254712111,0.));
#17291=CARTESIAN_POINT('Ctrl Pts',(13.1030026646917,15.5371254712111,21.));
#17292=CARTESIAN_POINT('Ctrl Pts',(13.1179844917497,15.5844317820184,0.));
#17293=CARTESIAN_POINT('Ctrl Pts',(13.1179844917497,15.5844317820184,21.));
#17294=CARTESIAN_POINT('Ctrl Pts',(13.1326905726717,15.6319054413079,0.));
#17295=CARTESIAN_POINT('Ctrl Pts',(13.1326905726717,15.6319054413079,21.));
#17296=CARTESIAN_POINT('Ctrl Pts',(13.147124558532,15.6795425955901,0.));
#17297=CARTESIAN_POINT('Ctrl Pts',(13.147124558532,15.6795425955901,21.));
#17298=CARTESIAN_POINT('Ctrl Pts',(13.161288914421,15.7273402954914,0.));
#17299=CARTESIAN_POINT('Ctrl Pts',(13.161288914421,15.7273402954914,21.));
#17300=CARTESIAN_POINT('Ctrl Pts',(13.1751853728467,15.7752961549278,0.));
#17301=CARTESIAN_POINT('Ctrl Pts',(13.1751853728467,15.7752961549278,21.));
#17302=CARTESIAN_POINT('Ctrl Pts',(13.1888152101588,15.8234081427091,0.));
#17303=CARTESIAN_POINT('Ctrl Pts',(13.1888152101588,15.8234081427091,21.));
#17304=CARTESIAN_POINT('Ctrl Pts',(13.2021795724682,15.8716743375555,0.));
#17305=CARTESIAN_POINT('Ctrl Pts',(13.2021795724682,15.8716743375555,21.));
#17306=CARTESIAN_POINT('Ctrl Pts',(13.2152798388134,15.9200926550954,0.));
#17307=CARTESIAN_POINT('Ctrl Pts',(13.2152798388134,15.9200926550954,21.));
#17308=CARTESIAN_POINT('Ctrl Pts',(13.2281177675127,15.9686607385389,0.));
#17309=CARTESIAN_POINT('Ctrl Pts',(13.2281177675127,15.9686607385389,21.));
#17310=CARTESIAN_POINT('Ctrl Pts',(13.240695304984,16.0173761036734,0.));
#17311=CARTESIAN_POINT('Ctrl Pts',(13.240695304984,16.0173761036734,21.));
#17312=CARTESIAN_POINT('Ctrl Pts',(13.2530144750236,16.0662362238032,0.));
#17313=CARTESIAN_POINT('Ctrl Pts',(13.2530144750236,16.0662362238032,21.));
#17314=CARTESIAN_POINT('Ctrl Pts',(13.2650772466062,16.1152386305152,0.));
#17315=CARTESIAN_POINT('Ctrl Pts',(13.2650772466062,16.1152386305152,21.));
#17316=CARTESIAN_POINT('Ctrl Pts',(13.2768853909882,16.1643810242643,0.));
#17317=CARTESIAN_POINT('Ctrl Pts',(13.2768853909882,16.1643810242643,21.));
#17318=CARTESIAN_POINT('Ctrl Pts',(13.2884404210388,16.2136613184475,0.));
#17319=CARTESIAN_POINT('Ctrl Pts',(13.2884404210388,16.2136613184475,21.));
#17320=CARTESIAN_POINT('Ctrl Pts',(13.2997436744733,16.2630775678735,0.));
#17321=CARTESIAN_POINT('Ctrl Pts',(13.2997436744733,16.2630775678735,21.));
#17322=CARTESIAN_POINT('Ctrl Pts',(13.3107963665229,16.3126279218067,0.));
#17323=CARTESIAN_POINT('Ctrl Pts',(13.3107963665229,16.3126279218067,21.));
#17324=CARTESIAN_POINT('Ctrl Pts',(13.3215996524974,16.3623105703343,0.));
#17325=CARTESIAN_POINT('Ctrl Pts',(13.3215996524974,16.3623105703343,21.));
#17326=CARTESIAN_POINT('Ctrl Pts',(13.3321546976812,16.4121236828756,0.));
#17327=CARTESIAN_POINT('Ctrl Pts',(13.3321546976812,16.4121236828756,21.));
#17328=CARTESIAN_POINT('Ctrl Pts',(13.3424627129921,16.4620653818862,0.));
#17329=CARTESIAN_POINT('Ctrl Pts',(13.3424627129921,16.4620653818862,21.));
#17330=CARTESIAN_POINT('Ctrl Pts',(13.3525249163084,16.5121337902953,0.));
#17331=CARTESIAN_POINT('Ctrl Pts',(13.3525249163084,16.5121337902953,21.));
#17332=CARTESIAN_POINT('Ctrl Pts',(13.3623425108873,16.5623270636327,0.));
#17333=CARTESIAN_POINT('Ctrl Pts',(13.3623425108873,16.5623270636327,21.));
#17334=CARTESIAN_POINT('Ctrl Pts',(13.3719166600676,16.612643424234,0.));
#17335=CARTESIAN_POINT('Ctrl Pts',(13.3719166600676,16.612643424234,21.));
#17336=CARTESIAN_POINT('Ctrl Pts',(13.381248462113,16.6630812012276,0.));
#17337=CARTESIAN_POINT('Ctrl Pts',(13.381248462113,16.6630812012276,21.));
#17338=CARTESIAN_POINT('Ctrl Pts',(13.3903389370346,16.7136388432444,0.));
#17339=CARTESIAN_POINT('Ctrl Pts',(13.3903389370346,16.7136388432444,21.));
#17340=CARTESIAN_POINT('Ctrl Pts',(13.3991890464165,16.7643148579873,0.));
#17341=CARTESIAN_POINT('Ctrl Pts',(13.3991890464165,16.7643148579873,21.));
#17342=CARTESIAN_POINT('Ctrl Pts',(13.4077997088426,16.8151077630226,0.));
#17343=CARTESIAN_POINT('Ctrl Pts',(13.4077997088426,16.8151077630226,21.));
#17344=CARTESIAN_POINT('Ctrl Pts',(13.4161718177499,16.8660160353187,0.));
#17345=CARTESIAN_POINT('Ctrl Pts',(13.4161718177499,16.8660160353187,21.));
#17346=CARTESIAN_POINT('Ctrl Pts',(13.4243062623592,16.9170380509036,0.));
#17347=CARTESIAN_POINT('Ctrl Pts',(13.4243062623592,16.9170380509036,21.));
#17348=CARTESIAN_POINT('Ctrl Pts',(13.432203941793,16.9681720567298,0.));
#17349=CARTESIAN_POINT('Ctrl Pts',(13.432203941793,16.9681720567298,21.));
#17350=CARTESIAN_POINT('Ctrl Pts',(13.4398657451291,17.0194162803447,0.));
#17351=CARTESIAN_POINT('Ctrl Pts',(13.4398657451291,17.0194162803447,21.));
#17352=CARTESIAN_POINT('Ctrl Pts',(13.4472925380889,17.0707690194412,0.));
#17353=CARTESIAN_POINT('Ctrl Pts',(13.4472925380889,17.0707690194412,21.));
#17354=CARTESIAN_POINT('Ctrl Pts',(13.4544851484583,17.1222287365697,0.));
#17355=CARTESIAN_POINT('Ctrl Pts',(13.4544851484583,17.1222287365697,21.));
#17356=CARTESIAN_POINT('Ctrl Pts',(13.4614443545811,17.173794155624,0.));
#17357=CARTESIAN_POINT('Ctrl Pts',(13.4614443545811,17.173794155624,21.));
#17358=CARTESIAN_POINT('Ctrl Pts',(13.4681708717969,17.2254643437923,0.));
#17359=CARTESIAN_POINT('Ctrl Pts',(13.4681708717969,17.2254643437923,21.));
#17360=CARTESIAN_POINT('Ctrl Pts',(13.474665315482,17.2772386565028,0.));
#17361=CARTESIAN_POINT('Ctrl Pts',(13.474665315482,17.2772386565028,21.));
#17362=CARTESIAN_POINT('Ctrl Pts',(13.4796755969465,17.3187410868027,0.));
#17363=CARTESIAN_POINT('Ctrl Pts',(13.4796755969465,17.3187410868027,21.));
#17364=CARTESIAN_POINT('Ctrl Pts',(13.4833292332349,17.3499144948292,0.));
#17365=CARTESIAN_POINT('Ctrl Pts',(13.4833292332349,17.3499144948292,21.));
#17366=CARTESIAN_POINT('Ctrl Pts',(13.485718750657,17.3707174645609,0.));
#17367=CARTESIAN_POINT('Ctrl Pts',(13.485718750657,17.3707174645609,21.));
#17368=CARTESIAN_POINT('Ctrl Pts',(13.4869019493419,17.3811241238545,0.));
#17369=CARTESIAN_POINT('Ctrl Pts',(13.4869019493419,17.3811241238545,21.));
#17370=CARTESIAN_POINT('Ctrl Pts',(12.4172651441477,14.1074595503134,0.));
#17371=CARTESIAN_POINT('Ctrl Pts',(12.4234926340671,14.1145347042316,0.));
#17372=CARTESIAN_POINT('Ctrl Pts',(12.4357509724316,14.1288394445866,0.));
#17373=CARTESIAN_POINT('Ctrl Pts',(12.4535485619996,14.1507598477672,0.));
#17374=CARTESIAN_POINT('Ctrl Pts',(12.4761570639125,14.1808688343892,0.));
#17375=CARTESIAN_POINT('Ctrl Pts',(12.5028859651751,14.2197144660135,0.));
#17376=CARTESIAN_POINT('Ctrl Pts',(12.5285125321527,14.2594378207584,0.));
#17377=CARTESIAN_POINT('Ctrl Pts',(12.5534605602317,14.2997103098726,0.));
#17378=CARTESIAN_POINT('Ctrl Pts',(12.5780443898087,14.3402859058353,0.));
#17379=CARTESIAN_POINT('Ctrl Pts',(12.6023830189244,14.3810669346235,0.));
#17380=CARTESIAN_POINT('Ctrl Pts',(12.626464614311,14.4220553460485,0.));
#17381=CARTESIAN_POINT('Ctrl Pts',(12.6501984687124,14.463313553928,0.));
#17382=CARTESIAN_POINT('Ctrl Pts',(12.6734695081852,14.5049233087958,0.));
#17383=CARTESIAN_POINT('Ctrl Pts',(12.6961966430455,14.5469417071951,0.));
#17384=CARTESIAN_POINT('Ctrl Pts',(12.7183743139638,14.5893698147583,0.));
#17385=CARTESIAN_POINT('Ctrl Pts',(12.7400427996251,14.6321748083434,0.));
#17386=CARTESIAN_POINT('Ctrl Pts',(12.7612687078867,14.6753044633399,0.));
#17387=CARTESIAN_POINT('Ctrl Pts',(12.7821227233337,14.7187037124277,0.));
#17388=CARTESIAN_POINT('Ctrl Pts',(12.8026557145457,14.7623324139791,0.));
#17389=CARTESIAN_POINT('Ctrl Pts',(12.8228846016791,14.8061758577898,0.));
#17390=CARTESIAN_POINT('Ctrl Pts',(12.8428057266944,14.8502347891476,0.));
#17391=CARTESIAN_POINT('Ctrl Pts',(12.8624032236317,14.8945191569251,0.));
#17392=CARTESIAN_POINT('Ctrl Pts',(12.8816587472147,14.9390408507356,0.));
#17393=CARTESIAN_POINT('Ctrl Pts',(12.9005620742036,14.9838057866976,0.));
#17394=CARTESIAN_POINT('Ctrl Pts',(12.9191164383568,15.0288099208306,0.));
#17395=CARTESIAN_POINT('Ctrl Pts',(12.9373327960422,15.0740435169624,0.));
#17396=CARTESIAN_POINT('Ctrl Pts',(12.9552263908864,15.1194937003528,0.));
#17397=CARTESIAN_POINT('Ctrl Pts',(12.9728126886697,15.1651474813659,0.));
#17398=CARTESIAN_POINT('Ctrl Pts',(12.9901029059182,15.2109950816083,0.));
#17399=CARTESIAN_POINT('Ctrl Pts',(13.0071020851025,15.2570313635503,0.));
#17400=CARTESIAN_POINT('Ctrl Pts',(13.0238115816728,15.3032539741328,0.));
#17401=CARTESIAN_POINT('Ctrl Pts',(13.0402305665115,15.3496622219036,0.));
#17402=CARTESIAN_POINT('Ctrl Pts',(13.0563577967298,15.3962557545684,0.));
#17403=CARTESIAN_POINT('Ctrl Pts',(13.0721935806302,15.4430330918328,0.));
#17404=CARTESIAN_POINT('Ctrl Pts',(13.087740560189,15.4899910401523,0.));
#17405=CARTESIAN_POINT('Ctrl Pts',(13.1030026646917,15.5371254712111,0.));
#17406=CARTESIAN_POINT('Ctrl Pts',(13.1179844917497,15.5844317820184,0.));
#17407=CARTESIAN_POINT('Ctrl Pts',(13.1326905726717,15.6319054413079,0.));
#17408=CARTESIAN_POINT('Ctrl Pts',(13.147124558532,15.6795425955901,0.));
#17409=CARTESIAN_POINT('Ctrl Pts',(13.161288914421,15.7273402954914,0.));
#17410=CARTESIAN_POINT('Ctrl Pts',(13.1751853728467,15.7752961549278,0.));
#17411=CARTESIAN_POINT('Ctrl Pts',(13.1888152101588,15.8234081427091,0.));
#17412=CARTESIAN_POINT('Ctrl Pts',(13.2021795724682,15.8716743375555,0.));
#17413=CARTESIAN_POINT('Ctrl Pts',(13.2152798388134,15.9200926550954,0.));
#17414=CARTESIAN_POINT('Ctrl Pts',(13.2281177675127,15.9686607385389,0.));
#17415=CARTESIAN_POINT('Ctrl Pts',(13.240695304984,16.0173761036734,0.));
#17416=CARTESIAN_POINT('Ctrl Pts',(13.2530144750236,16.0662362238032,0.));
#17417=CARTESIAN_POINT('Ctrl Pts',(13.2650772466062,16.1152386305152,0.));
#17418=CARTESIAN_POINT('Ctrl Pts',(13.2768853909882,16.1643810242643,0.));
#17419=CARTESIAN_POINT('Ctrl Pts',(13.2884404210388,16.2136613184475,0.));
#17420=CARTESIAN_POINT('Ctrl Pts',(13.2997436744733,16.2630775678735,0.));
#17421=CARTESIAN_POINT('Ctrl Pts',(13.3107963665229,16.3126279218067,0.));
#17422=CARTESIAN_POINT('Ctrl Pts',(13.3215996524974,16.3623105703343,0.));
#17423=CARTESIAN_POINT('Ctrl Pts',(13.3321546976812,16.4121236828756,0.));
#17424=CARTESIAN_POINT('Ctrl Pts',(13.3424627129921,16.4620653818862,0.));
#17425=CARTESIAN_POINT('Ctrl Pts',(13.3525249163084,16.5121337902953,0.));
#17426=CARTESIAN_POINT('Ctrl Pts',(13.3623425108873,16.5623270636327,0.));
#17427=CARTESIAN_POINT('Ctrl Pts',(13.3719166600676,16.612643424234,0.));
#17428=CARTESIAN_POINT('Ctrl Pts',(13.381248462113,16.6630812012276,0.));
#17429=CARTESIAN_POINT('Ctrl Pts',(13.3903389370346,16.7136388432444,0.));
#17430=CARTESIAN_POINT('Ctrl Pts',(13.3991890464165,16.7643148579873,0.));
#17431=CARTESIAN_POINT('Ctrl Pts',(13.4077997088426,16.8151077630226,0.));
#17432=CARTESIAN_POINT('Ctrl Pts',(13.4161718177499,16.8660160353187,0.));
#17433=CARTESIAN_POINT('Ctrl Pts',(13.4243062623592,16.9170380509036,0.));
#17434=CARTESIAN_POINT('Ctrl Pts',(13.432203941793,16.9681720567298,0.));
#17435=CARTESIAN_POINT('Ctrl Pts',(13.4398657451291,17.0194162803447,0.));
#17436=CARTESIAN_POINT('Ctrl Pts',(13.4472925380889,17.0707690194412,0.));
#17437=CARTESIAN_POINT('Ctrl Pts',(13.4544851484583,17.1222287365697,0.));
#17438=CARTESIAN_POINT('Ctrl Pts',(13.4614443545811,17.173794155624,0.));
#17439=CARTESIAN_POINT('Ctrl Pts',(13.4695161752401,17.235798381426,0.));
#17440=CARTESIAN_POINT('Ctrl Pts',(13.4759526005425,17.287598725272,0.));
#17441=CARTESIAN_POINT('Ctrl Pts',(13.4809165957478,17.3291218739796,0.));
#17442=CARTESIAN_POINT('Ctrl Pts',(13.4845355519784,17.360310805254,0.));
#17443=CARTESIAN_POINT('Ctrl Pts',(13.4869019493419,17.3811241238545,0.));
#17444=CARTESIAN_POINT('Ctrl Pts',(12.4172651441477,14.1074595503134,13.));
#17445=CARTESIAN_POINT('Ctrl Pts',(12.4277613166149,14.1193844248164,13.));
#17446=CARTESIAN_POINT('Ctrl Pts',(12.4379186757848,14.1315753314249,13.));
#17447=CARTESIAN_POINT('Ctrl Pts',(12.4477599775084,14.14401474732,13.));
#17448=CARTESIAN_POINT('Ctrl Pts',(12.45929471922,14.1585946731696,13.));
#17449=CARTESIAN_POINT('Ctrl Pts',(12.4703959522577,14.1735154808295,13.));
#17450=CARTESIAN_POINT('Ctrl Pts',(12.4811568677436,14.1887053040703,13.));
#17451=CARTESIAN_POINT('Ctrl Pts',(12.4962979908344,14.2100781123335,13.));
#17452=CARTESIAN_POINT('Ctrl Pts',(12.5107710847127,14.2319791941756,13.));
#17453=CARTESIAN_POINT('Ctrl Pts',(12.5249003586941,14.254157574695,13.));
#17454=CARTESIAN_POINT('Ctrl Pts',(12.5342985542355,14.2689096955178,13.));
#17455=CARTESIAN_POINT('Ctrl Pts',(12.5435462296413,14.2837832480516,13.));
#17456=CARTESIAN_POINT('Ctrl Pts',(12.5527146050322,14.298722508524,13.));
#17457=CARTESIAN_POINT('Ctrl Pts',(12.5623658230416,14.3144485290642,13.));
#17458=CARTESIAN_POINT('Ctrl Pts',(12.5719298675028,14.330246820686,13.));
#17459=CARTESIAN_POINT('Ctrl Pts',(12.5814385821519,14.3460912752807,13.));
#17460=CARTESIAN_POINT('Ctrl Pts',(12.5919985302804,14.3636874094394,13.));
#17461=CARTESIAN_POINT('Ctrl Pts',(12.6024891912727,14.381341260665,13.));
#17462=CARTESIAN_POINT('Ctrl Pts',(12.6128991700701,14.3990589912032,13.));
#17463=CARTESIAN_POINT('Ctrl Pts',(12.6285927183677,14.4257693299403,13.));
#17464=CARTESIAN_POINT('Ctrl Pts',(12.6440977931351,14.452628589856,13.));
#17465=CARTESIAN_POINT('Ctrl Pts',(12.6592867998067,14.4797266308813,13.));
#17466=CARTESIAN_POINT('Ctrl Pts',(12.6703212810873,14.4994127652612,13.));
#17467=CARTESIAN_POINT('Ctrl Pts',(12.6811863451307,14.5192269386383,13.));
#17468=CARTESIAN_POINT('Ctrl Pts',(12.6918647171384,14.5391805041508,13.));
#17469=CARTESIAN_POINT('Ctrl Pts',(12.7049181125412,14.5635720293893,13.));
#17470=CARTESIAN_POINT('Ctrl Pts',(12.7176935524276,14.5881710816651,13.));
#17471=CARTESIAN_POINT('Ctrl Pts',(12.7302281821981,14.612947560673,13.));
#17472=CARTESIAN_POINT('Ctrl Pts',(12.7437676626773,14.6397102700639,13.));
#17473=CARTESIAN_POINT('Ctrl Pts',(12.7570309720221,14.6666764215902,13.));
#17474=CARTESIAN_POINT('Ctrl Pts',(12.7700903554915,14.6937895363403,13.));
#17475=CARTESIAN_POINT('Ctrl Pts',(12.7821467169645,14.7188202365146,13.));
#17476=CARTESIAN_POINT('Ctrl Pts',(12.7940312932615,14.7439746960234,13.));
#17477=CARTESIAN_POINT('Ctrl Pts',(12.8057660290113,14.7692347187417,13.));
#17478=CARTESIAN_POINT('Ctrl Pts',(12.8217082700361,14.8035517565561,13.));
#17479=CARTESIAN_POINT('Ctrl Pts',(12.8373723698026,14.8380647951195,13.));
#17480=CARTESIAN_POINT('Ctrl Pts',(12.8527323828633,14.8727890594696,13.));
#17481=CARTESIAN_POINT('Ctrl Pts',(12.8675544637349,14.9062972246236,13.));
#17482=CARTESIAN_POINT('Ctrl Pts',(12.8820871276608,14.940006753605,13.));
#17483=CARTESIAN_POINT('Ctrl Pts',(12.8963159096104,14.9739251233869,13.));
#17484=CARTESIAN_POINT('Ctrl Pts',(12.9156461084297,15.0200041787713,13.));
#17485=CARTESIAN_POINT('Ctrl Pts',(12.9344180544732,15.0664667162891,13.));
#17486=CARTESIAN_POINT('Ctrl Pts',(12.9526968521391,15.113256758699,13.));
#17487=CARTESIAN_POINT('Ctrl Pts',(12.9687635180149,15.1543841890393,13.));
#17488=CARTESIAN_POINT('Ctrl Pts',(12.9844546719612,15.1957605758326,13.));
#17489=CARTESIAN_POINT('Ctrl Pts',(12.999793846462,15.2373637638652,13.));
#17490=CARTESIAN_POINT('Ctrl Pts',(13.0224075138868,15.2986969638966,13.));
#17491=CARTESIAN_POINT('Ctrl Pts',(13.0442489122257,15.3605284720897,13.));
#17492=CARTESIAN_POINT('Ctrl Pts',(13.0653151028224,15.4228468914086,13.));
#17493=CARTESIAN_POINT('Ctrl Pts',(13.0919008408212,15.5014933444024,13.));
#17494=CARTESIAN_POINT('Ctrl Pts',(13.1172560779922,15.5809121483295,13.));
#17495=CARTESIAN_POINT('Ctrl Pts',(13.1414683121752,15.6610132193997,13.));
#17496=CARTESIAN_POINT('Ctrl Pts',(13.1742656500619,15.7695162957013,13.));
#17497=CARTESIAN_POINT('Ctrl Pts',(13.2049609859129,15.8792747460677,13.));
#17498=CARTESIAN_POINT('Ctrl Pts',(13.2336341230255,15.9901726543658,13.));
#17499=CARTESIAN_POINT('Ctrl Pts',(13.2591969755608,16.0890410434498,13.));
#17500=CARTESIAN_POINT('Ctrl Pts',(13.2831593507059,16.1888100045206,13.));
#17501=CARTESIAN_POINT('Ctrl Pts',(13.3055799353303,16.2893994154296,13.));
#17502=CARTESIAN_POINT('Ctrl Pts',(13.3373560689398,16.4319622706935,13.));
#17503=CARTESIAN_POINT('Ctrl Pts',(13.3660302358948,16.576175723372,13.));
#17504=CARTESIAN_POINT('Ctrl Pts',(13.3917254914339,16.7218506169446,13.));
#17505=CARTESIAN_POINT('Ctrl Pts',(13.4116849578761,16.8350074269757,13.));
#17506=CARTESIAN_POINT('Ctrl Pts',(13.4298451931126,16.9490507057181,13.));
#17507=CARTESIAN_POINT('Ctrl Pts',(13.4462507328471,17.0638967767752,13.));
#17508=CARTESIAN_POINT('Ctrl Pts',(13.4604427660419,17.163247318062,13.));
#17509=CARTESIAN_POINT('Ctrl Pts',(13.4733230165186,17.2631945724315,13.));
#17510=CARTESIAN_POINT('Ctrl Pts',(13.4849093842842,17.3637184372217,13.));
#17511=CARTESIAN_POINT('Ctrl Pts',(13.4855778874128,17.3695184014096,13.));
#17512=CARTESIAN_POINT('Ctrl Pts',(13.4862420756862,17.3753202969914,13.));
#17513=CARTESIAN_POINT('Ctrl Pts',(13.4869019493419,17.3811241238545,13.));
#17514=CARTESIAN_POINT('Ctrl Pts',(17.3811241238545,13.4869019493419,0.));
#17515=CARTESIAN_POINT('Ctrl Pts',(17.3811241238545,13.4869019493419,21.));
#17516=CARTESIAN_POINT('Ctrl Pts',(17.3707174645609,13.485718750657,0.));
#17517=CARTESIAN_POINT('Ctrl Pts',(17.3707174645609,13.485718750657,21.));
#17518=CARTESIAN_POINT('Ctrl Pts',(17.3499144948292,13.4833292332349,0.));
#17519=CARTESIAN_POINT('Ctrl Pts',(17.3499144948292,13.4833292332349,21.));
#17520=CARTESIAN_POINT('Ctrl Pts',(17.3187410868027,13.4796755969465,0.));
#17521=CARTESIAN_POINT('Ctrl Pts',(17.3187410868027,13.4796755969465,21.));
#17522=CARTESIAN_POINT('Ctrl Pts',(17.2772386565028,13.474665315482,0.));
#17523=CARTESIAN_POINT('Ctrl Pts',(17.2772386565028,13.474665315482,21.));
#17524=CARTESIAN_POINT('Ctrl Pts',(17.2254643437923,13.4681708717969,0.));
#17525=CARTESIAN_POINT('Ctrl Pts',(17.2254643437923,13.4681708717969,21.));
#17526=CARTESIAN_POINT('Ctrl Pts',(17.173794155624,13.4614443545811,0.));
#17527=CARTESIAN_POINT('Ctrl Pts',(17.173794155624,13.4614443545811,21.));
#17528=CARTESIAN_POINT('Ctrl Pts',(17.1222287365697,13.4544851484583,0.));
#17529=CARTESIAN_POINT('Ctrl Pts',(17.1222287365697,13.4544851484583,21.));
#17530=CARTESIAN_POINT('Ctrl Pts',(17.0707690194411,13.4472925380889,0.));
#17531=CARTESIAN_POINT('Ctrl Pts',(17.0707690194411,13.4472925380889,21.));
#17532=CARTESIAN_POINT('Ctrl Pts',(17.0194162803447,13.4398657451291,0.));
#17533=CARTESIAN_POINT('Ctrl Pts',(17.0194162803447,13.4398657451291,21.));
#17534=CARTESIAN_POINT('Ctrl Pts',(16.9681720567298,13.432203941793,0.));
#17535=CARTESIAN_POINT('Ctrl Pts',(16.9681720567298,13.432203941793,21.));
#17536=CARTESIAN_POINT('Ctrl Pts',(16.9170380509036,13.4243062623592,0.));
#17537=CARTESIAN_POINT('Ctrl Pts',(16.9170380509036,13.4243062623592,21.));
#17538=CARTESIAN_POINT('Ctrl Pts',(16.8660160353187,13.4161718177499,0.));
#17539=CARTESIAN_POINT('Ctrl Pts',(16.8660160353187,13.4161718177499,21.));
#17540=CARTESIAN_POINT('Ctrl Pts',(16.8151077630226,13.4077997088426,0.));
#17541=CARTESIAN_POINT('Ctrl Pts',(16.8151077630226,13.4077997088426,21.));
#17542=CARTESIAN_POINT('Ctrl Pts',(16.7643148579873,13.3991890464165,0.));
#17543=CARTESIAN_POINT('Ctrl Pts',(16.7643148579873,13.3991890464165,21.));
#17544=CARTESIAN_POINT('Ctrl Pts',(16.7136388432444,13.3903389370346,0.));
#17545=CARTESIAN_POINT('Ctrl Pts',(16.7136388432444,13.3903389370346,21.));
#17546=CARTESIAN_POINT('Ctrl Pts',(16.6630812012276,13.381248462113,0.));
#17547=CARTESIAN_POINT('Ctrl Pts',(16.6630812012276,13.381248462113,21.));
#17548=CARTESIAN_POINT('Ctrl Pts',(16.612643424234,13.3719166600676,0.));
#17549=CARTESIAN_POINT('Ctrl Pts',(16.612643424234,13.3719166600676,21.));
#17550=CARTESIAN_POINT('Ctrl Pts',(16.5623270636327,13.3623425108873,0.));
#17551=CARTESIAN_POINT('Ctrl Pts',(16.5623270636327,13.3623425108873,21.));
#17552=CARTESIAN_POINT('Ctrl Pts',(16.5121337902953,13.3525249163084,0.));
#17553=CARTESIAN_POINT('Ctrl Pts',(16.5121337902953,13.3525249163084,21.));
#17554=CARTESIAN_POINT('Ctrl Pts',(16.4620653818862,13.3424627129921,0.));
#17555=CARTESIAN_POINT('Ctrl Pts',(16.4620653818862,13.3424627129921,21.));
#17556=CARTESIAN_POINT('Ctrl Pts',(16.4121236828756,13.3321546976812,0.));
#17557=CARTESIAN_POINT('Ctrl Pts',(16.4121236828756,13.3321546976812,21.));
#17558=CARTESIAN_POINT('Ctrl Pts',(16.3623105703343,13.3215996524974,0.));
#17559=CARTESIAN_POINT('Ctrl Pts',(16.3623105703343,13.3215996524974,21.));
#17560=CARTESIAN_POINT('Ctrl Pts',(16.3126279218067,13.3107963665229,0.));
#17561=CARTESIAN_POINT('Ctrl Pts',(16.3126279218067,13.3107963665229,21.));
#17562=CARTESIAN_POINT('Ctrl Pts',(16.2630775678735,13.2997436744733,0.));
#17563=CARTESIAN_POINT('Ctrl Pts',(16.2630775678735,13.2997436744733,21.));
#17564=CARTESIAN_POINT('Ctrl Pts',(16.2136613184475,13.2884404210387,0.));
#17565=CARTESIAN_POINT('Ctrl Pts',(16.2136613184475,13.2884404210387,21.));
#17566=CARTESIAN_POINT('Ctrl Pts',(16.1643810242643,13.2768853909882,0.));
#17567=CARTESIAN_POINT('Ctrl Pts',(16.1643810242643,13.2768853909882,21.));
#17568=CARTESIAN_POINT('Ctrl Pts',(16.1152386305152,13.2650772466062,0.));
#17569=CARTESIAN_POINT('Ctrl Pts',(16.1152386305152,13.2650772466062,21.));
#17570=CARTESIAN_POINT('Ctrl Pts',(16.0662362238032,13.2530144750236,0.));
#17571=CARTESIAN_POINT('Ctrl Pts',(16.0662362238032,13.2530144750236,21.));
#17572=CARTESIAN_POINT('Ctrl Pts',(16.0173761036734,13.240695304984,0.));
#17573=CARTESIAN_POINT('Ctrl Pts',(16.0173761036734,13.240695304984,21.));
#17574=CARTESIAN_POINT('Ctrl Pts',(15.9686607385389,13.2281177675127,0.));
#17575=CARTESIAN_POINT('Ctrl Pts',(15.9686607385389,13.2281177675127,21.));
#17576=CARTESIAN_POINT('Ctrl Pts',(15.9200926550954,13.2152798388134,0.));
#17577=CARTESIAN_POINT('Ctrl Pts',(15.9200926550954,13.2152798388134,21.));
#17578=CARTESIAN_POINT('Ctrl Pts',(15.8716743375555,13.2021795724682,0.));
#17579=CARTESIAN_POINT('Ctrl Pts',(15.8716743375555,13.2021795724682,21.));
#17580=CARTESIAN_POINT('Ctrl Pts',(15.8234081427091,13.1888152101588,0.));
#17581=CARTESIAN_POINT('Ctrl Pts',(15.8234081427091,13.1888152101588,21.));
#17582=CARTESIAN_POINT('Ctrl Pts',(15.7752961549278,13.1751853728467,0.));
#17583=CARTESIAN_POINT('Ctrl Pts',(15.7752961549278,13.1751853728467,21.));
#17584=CARTESIAN_POINT('Ctrl Pts',(15.7273402954914,13.161288914421,0.));
#17585=CARTESIAN_POINT('Ctrl Pts',(15.7273402954914,13.161288914421,21.));
#17586=CARTESIAN_POINT('Ctrl Pts',(15.6795425955901,13.147124558532,0.));
#17587=CARTESIAN_POINT('Ctrl Pts',(15.6795425955901,13.147124558532,21.));
#17588=CARTESIAN_POINT('Ctrl Pts',(15.6319054413079,13.1326905726717,0.));
#17589=CARTESIAN_POINT('Ctrl Pts',(15.6319054413079,13.1326905726717,21.));
#17590=CARTESIAN_POINT('Ctrl Pts',(15.5844317820184,13.1179844917497,0.));
#17591=CARTESIAN_POINT('Ctrl Pts',(15.5844317820184,13.1179844917497,21.));
#17592=CARTESIAN_POINT('Ctrl Pts',(15.5371254712111,13.1030026646917,0.));
#17593=CARTESIAN_POINT('Ctrl Pts',(15.5371254712111,13.1030026646917,21.));
#17594=CARTESIAN_POINT('Ctrl Pts',(15.4899910401523,13.087740560189,0.));
#17595=CARTESIAN_POINT('Ctrl Pts',(15.4899910401523,13.087740560189,21.));
#17596=CARTESIAN_POINT('Ctrl Pts',(15.4430330918328,13.0721935806302,0.));
#17597=CARTESIAN_POINT('Ctrl Pts',(15.4430330918328,13.0721935806302,21.));
#17598=CARTESIAN_POINT('Ctrl Pts',(15.3962557545684,13.0563577967298,0.));
#17599=CARTESIAN_POINT('Ctrl Pts',(15.3962557545684,13.0563577967298,21.));
#17600=CARTESIAN_POINT('Ctrl Pts',(15.3496622219036,13.0402305665115,0.));
#17601=CARTESIAN_POINT('Ctrl Pts',(15.3496622219036,13.0402305665115,21.));
#17602=CARTESIAN_POINT('Ctrl Pts',(15.3032539741328,13.0238115816728,0.));
#17603=CARTESIAN_POINT('Ctrl Pts',(15.3032539741328,13.0238115816728,21.));
#17604=CARTESIAN_POINT('Ctrl Pts',(15.2570313635503,13.0071020851025,0.));
#17605=CARTESIAN_POINT('Ctrl Pts',(15.2570313635503,13.0071020851025,21.));
#17606=CARTESIAN_POINT('Ctrl Pts',(15.2109950816083,12.9901029059182,0.));
#17607=CARTESIAN_POINT('Ctrl Pts',(15.2109950816083,12.9901029059182,21.));
#17608=CARTESIAN_POINT('Ctrl Pts',(15.1651474813659,12.9728126886697,0.));
#17609=CARTESIAN_POINT('Ctrl Pts',(15.1651474813659,12.9728126886697,21.));
#17610=CARTESIAN_POINT('Ctrl Pts',(15.1194937003528,12.9552263908864,0.));
#17611=CARTESIAN_POINT('Ctrl Pts',(15.1194937003528,12.9552263908864,21.));
#17612=CARTESIAN_POINT('Ctrl Pts',(15.0740435169624,12.9373327960422,0.));
#17613=CARTESIAN_POINT('Ctrl Pts',(15.0740435169624,12.9373327960422,21.));
#17614=CARTESIAN_POINT('Ctrl Pts',(15.0288099208306,12.9191164383568,0.));
#17615=CARTESIAN_POINT('Ctrl Pts',(15.0288099208306,12.9191164383568,21.));
#17616=CARTESIAN_POINT('Ctrl Pts',(14.9838057866976,12.9005620742036,0.));
#17617=CARTESIAN_POINT('Ctrl Pts',(14.9838057866976,12.9005620742036,21.));
#17618=CARTESIAN_POINT('Ctrl Pts',(14.9390408507356,12.8816587472147,0.));
#17619=CARTESIAN_POINT('Ctrl Pts',(14.9390408507356,12.8816587472147,21.));
#17620=CARTESIAN_POINT('Ctrl Pts',(14.8945191569251,12.8624032236317,0.));
#17621=CARTESIAN_POINT('Ctrl Pts',(14.8945191569251,12.8624032236317,21.));
#17622=CARTESIAN_POINT('Ctrl Pts',(14.8502347891476,12.8428057266944,0.));
#17623=CARTESIAN_POINT('Ctrl Pts',(14.8502347891476,12.8428057266944,21.));
#17624=CARTESIAN_POINT('Ctrl Pts',(14.8061758577898,12.8228846016791,0.));
#17625=CARTESIAN_POINT('Ctrl Pts',(14.8061758577898,12.8228846016791,21.));
#17626=CARTESIAN_POINT('Ctrl Pts',(14.7623324139791,12.8026557145457,0.));
#17627=CARTESIAN_POINT('Ctrl Pts',(14.7623324139791,12.8026557145457,21.));
#17628=CARTESIAN_POINT('Ctrl Pts',(14.7187037124277,12.7821227233337,0.));
#17629=CARTESIAN_POINT('Ctrl Pts',(14.7187037124277,12.7821227233337,21.));
#17630=CARTESIAN_POINT('Ctrl Pts',(14.6753044633399,12.7612687078867,0.));
#17631=CARTESIAN_POINT('Ctrl Pts',(14.6753044633399,12.7612687078867,21.));
#17632=CARTESIAN_POINT('Ctrl Pts',(14.6321748083434,12.7400427996251,0.));
#17633=CARTESIAN_POINT('Ctrl Pts',(14.6321748083434,12.7400427996251,21.));
#17634=CARTESIAN_POINT('Ctrl Pts',(14.5893698147583,12.7183743139638,0.));
#17635=CARTESIAN_POINT('Ctrl Pts',(14.5893698147583,12.7183743139638,21.));
#17636=CARTESIAN_POINT('Ctrl Pts',(14.5469417071951,12.6961966430455,0.));
#17637=CARTESIAN_POINT('Ctrl Pts',(14.5469417071951,12.6961966430455,21.));
#17638=CARTESIAN_POINT('Ctrl Pts',(14.5049233087958,12.6734695081852,0.));
#17639=CARTESIAN_POINT('Ctrl Pts',(14.5049233087958,12.6734695081852,21.));
#17640=CARTESIAN_POINT('Ctrl Pts',(14.463313553928,12.6501984687124,0.));
#17641=CARTESIAN_POINT('Ctrl Pts',(14.463313553928,12.6501984687124,21.));
#17642=CARTESIAN_POINT('Ctrl Pts',(14.4220553460485,12.626464614311,0.));
#17643=CARTESIAN_POINT('Ctrl Pts',(14.4220553460485,12.626464614311,21.));
#17644=CARTESIAN_POINT('Ctrl Pts',(14.3810669346235,12.6023830189244,0.));
#17645=CARTESIAN_POINT('Ctrl Pts',(14.3810669346235,12.6023830189244,21.));
#17646=CARTESIAN_POINT('Ctrl Pts',(14.3402859058353,12.5780443898087,0.));
#17647=CARTESIAN_POINT('Ctrl Pts',(14.3402859058353,12.5780443898087,21.));
#17648=CARTESIAN_POINT('Ctrl Pts',(14.2997103098726,12.5534605602317,0.));
#17649=CARTESIAN_POINT('Ctrl Pts',(14.2997103098726,12.5534605602317,21.));
#17650=CARTESIAN_POINT('Ctrl Pts',(14.2594378207584,12.5285125321527,0.));
#17651=CARTESIAN_POINT('Ctrl Pts',(14.2594378207584,12.5285125321527,21.));
#17652=CARTESIAN_POINT('Ctrl Pts',(14.2197144660135,12.502885965175,0.));
#17653=CARTESIAN_POINT('Ctrl Pts',(14.2197144660135,12.502885965175,21.));
#17654=CARTESIAN_POINT('Ctrl Pts',(14.1808688343892,12.4761570639125,0.));
#17655=CARTESIAN_POINT('Ctrl Pts',(14.1808688343892,12.4761570639125,21.));
#17656=CARTESIAN_POINT('Ctrl Pts',(14.1507598477672,12.4535485619996,0.));
#17657=CARTESIAN_POINT('Ctrl Pts',(14.1507598477672,12.4535485619996,21.));
#17658=CARTESIAN_POINT('Ctrl Pts',(14.1288394445866,12.4357509724316,0.));
#17659=CARTESIAN_POINT('Ctrl Pts',(14.1288394445866,12.4357509724316,21.));
#17660=CARTESIAN_POINT('Ctrl Pts',(14.1145347042316,12.4234926340671,0.));
#17661=CARTESIAN_POINT('Ctrl Pts',(14.1145347042316,12.4234926340671,21.));
#17662=CARTESIAN_POINT('Ctrl Pts',(14.1074595503134,12.4172651441477,0.));
#17663=CARTESIAN_POINT('Ctrl Pts',(14.1074595503134,12.4172651441477,21.));
#17664=CARTESIAN_POINT('',(17.3811241238545,13.486901949342,0.));
#17665=CARTESIAN_POINT('Ctrl Pts',(14.1074595503134,12.4172651441477,0.));
#17666=CARTESIAN_POINT('Ctrl Pts',(14.1145347042316,12.4234926340671,0.));
#17667=CARTESIAN_POINT('Ctrl Pts',(14.1288394445866,12.4357509724316,0.));
#17668=CARTESIAN_POINT('Ctrl Pts',(14.1507598477672,12.4535485619996,0.));
#17669=CARTESIAN_POINT('Ctrl Pts',(14.1808688343892,12.4761570639125,0.));
#17670=CARTESIAN_POINT('Ctrl Pts',(14.2197144660135,12.502885965175,0.));
#17671=CARTESIAN_POINT('Ctrl Pts',(14.2594378207584,12.5285125321527,0.));
#17672=CARTESIAN_POINT('Ctrl Pts',(14.2997103098726,12.5534605602317,0.));
#17673=CARTESIAN_POINT('Ctrl Pts',(14.3402859058353,12.5780443898087,0.));
#17674=CARTESIAN_POINT('Ctrl Pts',(14.3810669346235,12.6023830189244,0.));
#17675=CARTESIAN_POINT('Ctrl Pts',(14.4220553460485,12.626464614311,0.));
#17676=CARTESIAN_POINT('Ctrl Pts',(14.463313553928,12.6501984687124,0.));
#17677=CARTESIAN_POINT('Ctrl Pts',(14.5049233087958,12.6734695081852,0.));
#17678=CARTESIAN_POINT('Ctrl Pts',(14.5469417071951,12.6961966430455,0.));
#17679=CARTESIAN_POINT('Ctrl Pts',(14.5893698147583,12.7183743139638,0.));
#17680=CARTESIAN_POINT('Ctrl Pts',(14.6321748083434,12.7400427996251,0.));
#17681=CARTESIAN_POINT('Ctrl Pts',(14.6753044633399,12.7612687078867,0.));
#17682=CARTESIAN_POINT('Ctrl Pts',(14.7187037124277,12.7821227233337,0.));
#17683=CARTESIAN_POINT('Ctrl Pts',(14.7623324139791,12.8026557145457,0.));
#17684=CARTESIAN_POINT('Ctrl Pts',(14.8061758577898,12.8228846016791,0.));
#17685=CARTESIAN_POINT('Ctrl Pts',(14.8502347891476,12.8428057266944,0.));
#17686=CARTESIAN_POINT('Ctrl Pts',(14.8945191569251,12.8624032236317,0.));
#17687=CARTESIAN_POINT('Ctrl Pts',(14.9390408507356,12.8816587472147,0.));
#17688=CARTESIAN_POINT('Ctrl Pts',(14.9838057866976,12.9005620742036,0.));
#17689=CARTESIAN_POINT('Ctrl Pts',(15.0288099208306,12.9191164383568,0.));
#17690=CARTESIAN_POINT('Ctrl Pts',(15.0740435169624,12.9373327960422,0.));
#17691=CARTESIAN_POINT('Ctrl Pts',(15.1194937003528,12.9552263908864,0.));
#17692=CARTESIAN_POINT('Ctrl Pts',(15.1651474813659,12.9728126886697,0.));
#17693=CARTESIAN_POINT('Ctrl Pts',(15.2109950816083,12.9901029059182,0.));
#17694=CARTESIAN_POINT('Ctrl Pts',(15.2570313635503,13.0071020851025,0.));
#17695=CARTESIAN_POINT('Ctrl Pts',(15.3032539741328,13.0238115816728,0.));
#17696=CARTESIAN_POINT('Ctrl Pts',(15.3496622219036,13.0402305665115,0.));
#17697=CARTESIAN_POINT('Ctrl Pts',(15.3962557545684,13.0563577967298,0.));
#17698=CARTESIAN_POINT('Ctrl Pts',(15.4430330918328,13.0721935806302,0.));
#17699=CARTESIAN_POINT('Ctrl Pts',(15.4899910401523,13.087740560189,0.));
#17700=CARTESIAN_POINT('Ctrl Pts',(15.5371254712111,13.1030026646917,0.));
#17701=CARTESIAN_POINT('Ctrl Pts',(15.5844317820184,13.1179844917497,0.));
#17702=CARTESIAN_POINT('Ctrl Pts',(15.6319054413079,13.1326905726717,0.));
#17703=CARTESIAN_POINT('Ctrl Pts',(15.6795425955901,13.147124558532,0.));
#17704=CARTESIAN_POINT('Ctrl Pts',(15.7273402954914,13.161288914421,0.));
#17705=CARTESIAN_POINT('Ctrl Pts',(15.7752961549278,13.1751853728467,0.));
#17706=CARTESIAN_POINT('Ctrl Pts',(15.8234081427091,13.1888152101588,0.));
#17707=CARTESIAN_POINT('Ctrl Pts',(15.8716743375555,13.2021795724682,0.));
#17708=CARTESIAN_POINT('Ctrl Pts',(15.9200926550954,13.2152798388134,0.));
#17709=CARTESIAN_POINT('Ctrl Pts',(15.9686607385389,13.2281177675127,0.));
#17710=CARTESIAN_POINT('Ctrl Pts',(16.0173761036734,13.240695304984,0.));
#17711=CARTESIAN_POINT('Ctrl Pts',(16.0662362238032,13.2530144750236,0.));
#17712=CARTESIAN_POINT('Ctrl Pts',(16.1152386305152,13.2650772466062,0.));
#17713=CARTESIAN_POINT('Ctrl Pts',(16.1643810242643,13.2768853909882,0.));
#17714=CARTESIAN_POINT('Ctrl Pts',(16.2136613184475,13.2884404210387,0.));
#17715=CARTESIAN_POINT('Ctrl Pts',(16.2630775678735,13.2997436744733,0.));
#17716=CARTESIAN_POINT('Ctrl Pts',(16.3126279218067,13.3107963665229,0.));
#17717=CARTESIAN_POINT('Ctrl Pts',(16.3623105703343,13.3215996524974,0.));
#17718=CARTESIAN_POINT('Ctrl Pts',(16.4121236828756,13.3321546976812,0.));
#17719=CARTESIAN_POINT('Ctrl Pts',(16.4620653818862,13.3424627129921,0.));
#17720=CARTESIAN_POINT('Ctrl Pts',(16.5121337902953,13.3525249163084,0.));
#17721=CARTESIAN_POINT('Ctrl Pts',(16.5623270636327,13.3623425108873,0.));
#17722=CARTESIAN_POINT('Ctrl Pts',(16.612643424234,13.3719166600676,0.));
#17723=CARTESIAN_POINT('Ctrl Pts',(16.6630812012276,13.381248462113,0.));
#17724=CARTESIAN_POINT('Ctrl Pts',(16.7136388432444,13.3903389370346,0.));
#17725=CARTESIAN_POINT('Ctrl Pts',(16.7643148579873,13.3991890464165,0.));
#17726=CARTESIAN_POINT('Ctrl Pts',(16.8151077630226,13.4077997088426,0.));
#17727=CARTESIAN_POINT('Ctrl Pts',(16.8660160353187,13.4161718177499,0.));
#17728=CARTESIAN_POINT('Ctrl Pts',(16.9170380509036,13.4243062623592,0.));
#17729=CARTESIAN_POINT('Ctrl Pts',(16.9681720567298,13.432203941793,0.));
#17730=CARTESIAN_POINT('Ctrl Pts',(17.0194162803447,13.4398657451291,0.));
#17731=CARTESIAN_POINT('Ctrl Pts',(17.0707690194411,13.4472925380889,0.));
#17732=CARTESIAN_POINT('Ctrl Pts',(17.1222287365697,13.4544851484583,0.));
#17733=CARTESIAN_POINT('Ctrl Pts',(17.173794155624,13.4614443545811,0.));
#17734=CARTESIAN_POINT('Ctrl Pts',(17.235798381426,13.4695161752401,0.));
#17735=CARTESIAN_POINT('Ctrl Pts',(17.287598725272,13.4759526005425,0.));
#17736=CARTESIAN_POINT('Ctrl Pts',(17.3291218739796,13.4809165957478,0.));
#17737=CARTESIAN_POINT('Ctrl Pts',(17.360310805254,13.4845355519784,0.));
#17738=CARTESIAN_POINT('Ctrl Pts',(17.3811241238545,13.4869019493419,0.));
#17739=CARTESIAN_POINT('',(17.3811241238545,13.486901949342,13.));
#17740=CARTESIAN_POINT('Ctrl Pts',(17.3811241238545,13.4869019493419,13.));
#17741=CARTESIAN_POINT('Ctrl Pts',(17.2786694026925,13.475253226354,13.));
#17742=CARTESIAN_POINT('Ctrl Pts',(17.1768129075703,13.4622625504827,13.));
#17743=CARTESIAN_POINT('Ctrl Pts',(17.0755735571126,13.4479123002588,13.));
#17744=CARTESIAN_POINT('Ctrl Pts',(16.9078155789347,13.4241333155753,13.));
#17745=CARTESIAN_POINT('Ctrl Pts',(16.7417653345045,13.3966181288102,13.));
#17746=CARTESIAN_POINT('Ctrl Pts',(16.5776745323047,13.3652244057455,13.));
#17747=CARTESIAN_POINT('Ctrl Pts',(16.4515447193844,13.3410933492578,13.));
#17748=CARTESIAN_POINT('Ctrl Pts',(16.326570616418,13.3146689208721,13.));
#17749=CARTESIAN_POINT('Ctrl Pts',(16.2028831212964,13.285866517354,13.));
#17750=CARTESIAN_POINT('Ctrl Pts',(16.06973652377,13.2548614264574,13.));
#17751=CARTESIAN_POINT('Ctrl Pts',(15.9380763875928,13.2211052775845,13.));
#17752=CARTESIAN_POINT('Ctrl Pts',(15.8081115268615,13.1844379737316,13.));
#17753=CARTESIAN_POINT('Ctrl Pts',(15.7361594415553,13.1641379560196,13.));
#17754=CARTESIAN_POINT('Ctrl Pts',(15.6647240151602,13.1429498676482,13.));
#17755=CARTESIAN_POINT('Ctrl Pts',(15.5938437133287,13.1208442205595,13.));
#17756=CARTESIAN_POINT('Ctrl Pts',(15.5255406834836,13.0995423548249,13.));
#17757=CARTESIAN_POINT('Ctrl Pts',(15.4577571790122,13.0773830006569,13.));
#17758=CARTESIAN_POINT('Ctrl Pts',(15.3905488537597,13.0543129127178,13.));
#17759=CARTESIAN_POINT('Ctrl Pts',(15.332460243202,13.0343732795132,13.));
#17760=CARTESIAN_POINT('Ctrl Pts',(15.2747993571085,13.0137559282893,13.));
#17761=CARTESIAN_POINT('Ctrl Pts',(15.2175748360866,12.9924643454807,13.));
#17762=CARTESIAN_POINT('Ctrl Pts',(15.1765073868617,12.9771843399814,13.));
#17763=CARTESIAN_POINT('Ctrl Pts',(15.1356629994431,12.9615593596241,13.));
#17764=CARTESIAN_POINT('Ctrl Pts',(15.0950681393122,12.9455599550767,13.));
#17765=CARTESIAN_POINT('Ctrl Pts',(15.0551343146459,12.929821080404,13.));
#17766=CARTESIAN_POINT('Ctrl Pts',(15.0154457680865,12.9137147527836,13.));
#17767=CARTESIAN_POINT('Ctrl Pts',(14.9760367885877,12.8972012563026,13.));
#17768=CARTESIAN_POINT('Ctrl Pts',(14.9418668884515,12.8828830848393,13.));
#17769=CARTESIAN_POINT('Ctrl Pts',(14.9079086463149,12.8682568219259,13.));
#17770=CARTESIAN_POINT('Ctrl Pts',(14.8741550421669,12.8533364078128,13.));
#17771=CARTESIAN_POINT('Ctrl Pts',(14.8435820219545,12.8398219362837,13.));
#17772=CARTESIAN_POINT('Ctrl Pts',(14.8131735645768,12.8260705986513,13.));
#17773=CARTESIAN_POINT('Ctrl Pts',(14.7829174085775,12.812102575688,13.));
#17774=CARTESIAN_POINT('Ctrl Pts',(14.757431220614,12.8003366508055,13.));
#17775=CARTESIAN_POINT('Ctrl Pts',(14.7320520617549,12.7884183711613,13.));
#17776=CARTESIAN_POINT('Ctrl Pts',(14.7067929855474,12.7763327019834,13.));
#17777=CARTESIAN_POINT('Ctrl Pts',(14.670240352911,12.7588434231993,13.));
#17778=CARTESIAN_POINT('Ctrl Pts',(14.6339396294554,12.7410029356166,13.));
#17779=CARTESIAN_POINT('Ctrl Pts',(14.5980256541895,12.7226389621465,13.));
#17780=CARTESIAN_POINT('Ctrl Pts',(14.5763250378172,12.7115427373371,13.));
#17781=CARTESIAN_POINT('Ctrl Pts',(14.5547677202271,12.70025260105,13.));
#17782=CARTESIAN_POINT('Ctrl Pts',(14.533370542915,12.6887481999834,13.));
#17783=CARTESIAN_POINT('Ctrl Pts',(14.5136363259179,12.6781379057488,13.));
#17784=CARTESIAN_POINT('Ctrl Pts',(14.4940391165059,12.6673442955906,13.));
#17785=CARTESIAN_POINT('Ctrl Pts',(14.4745649061758,12.6563881737138,13.));
#17786=CARTESIAN_POINT('Ctrl Pts',(14.4477761570948,12.6413169181978,13.));
#17787=CARTESIAN_POINT('Ctrl Pts',(14.4212156950463,12.6259439377271,13.));
#17788=CARTESIAN_POINT('Ctrl Pts',(14.3947967979234,12.6103925840948,13.));
#17789=CARTESIAN_POINT('Ctrl Pts',(14.3780361778422,12.6005265276593,13.));
#17790=CARTESIAN_POINT('Ctrl Pts',(14.3613315560818,12.5905900369939,13.));
#17791=CARTESIAN_POINT('Ctrl Pts',(14.3446791499932,12.5805908895765,13.));
#17792=CARTESIAN_POINT('Ctrl Pts',(14.3297343906419,12.5716171201957,13.));
#17793=CARTESIAN_POINT('Ctrl Pts',(14.3148312513045,12.5625934693725,13.));
#17794=CARTESIAN_POINT('Ctrl Pts',(14.2999916562562,12.5534931963385,13.));
#17795=CARTESIAN_POINT('Ctrl Pts',(14.2843922864144,12.5439269969742,13.));
#17796=CARTESIAN_POINT('Ctrl Pts',(14.2688630441931,12.5342762591635,13.));
#17797=CARTESIAN_POINT('Ctrl Pts',(14.2534670739585,12.5244602884384,13.));
#17798=CARTESIAN_POINT('Ctrl Pts',(14.2278944013234,12.508155982693,13.));
#17799=CARTESIAN_POINT('Ctrl Pts',(14.2026946288202,12.4913891918572,13.));
#17800=CARTESIAN_POINT('Ctrl Pts',(14.1782508275394,12.4736648235789,13.));
#17801=CARTESIAN_POINT('Ctrl Pts',(14.1647716456173,12.4638909761427,13.));
#17802=CARTESIAN_POINT('Ctrl Pts',(14.1515231428256,12.4538248358964,13.));
#17803=CARTESIAN_POINT('Ctrl Pts',(14.1385523183786,12.4434054354823,13.));
#17804=CARTESIAN_POINT('Ctrl Pts',(14.1280012216095,12.4349297905843,13.));
#17805=CARTESIAN_POINT('Ctrl Pts',(14.1176338182992,12.4262204477427,13.));
#17806=CARTESIAN_POINT('Ctrl Pts',(14.1074595503134,12.4172651441477,13.));
#17807=CARTESIAN_POINT('',(17.3811241238545,13.486901949342,0.));
#17808=CARTESIAN_POINT('Origin',(4.58435815896522E-12,3.33073116609659E-12,
0.));
#17809=CARTESIAN_POINT('',(18.1978687191668,12.3627494547115,0.));
#17810=CARTESIAN_POINT('Origin',(4.58435815896522E-12,3.33073116609659E-12,
0.));
#17811=CARTESIAN_POINT('',(18.1978687191668,12.3627494547115,13.));
#17812=CARTESIAN_POINT('Origin',(4.58435815896522E-12,3.33073116609659E-12,
13.));
#17813=CARTESIAN_POINT('',(18.1978687191668,12.3627494547115,0.));
#17814=CARTESIAN_POINT('Ctrl Pts',(16.1689656784104,9.57984538049455,0.));
#17815=CARTESIAN_POINT('Ctrl Pts',(16.1689656784104,9.57984538049455,21.));
#17816=CARTESIAN_POINT('Ctrl Pts',(16.1770747160769,9.58464985151482,0.));
#17817=CARTESIAN_POINT('Ctrl Pts',(16.1770747160769,9.58464985151482,21.));
#17818=CARTESIAN_POINT('Ctrl Pts',(16.1931534965272,9.59446643316596,0.));
#17819=CARTESIAN_POINT('Ctrl Pts',(16.1931534965272,9.59446643316596,21.));
#17820=CARTESIAN_POINT('Ctrl Pts',(16.2168537871666,9.60981421781524,0.));
#17821=CARTESIAN_POINT('Ctrl Pts',(16.2168537871666,9.60981421781524,21.));
#17822=CARTESIAN_POINT('Ctrl Pts',(16.2476599387841,9.63146315443273,0.));
#17823=CARTESIAN_POINT('Ctrl Pts',(16.2476599387841,9.63146315443273,21.));
#17824=CARTESIAN_POINT('Ctrl Pts',(16.2850845948324,9.66014786078746,0.));
#17825=CARTESIAN_POINT('Ctrl Pts',(16.2850845948324,9.66014786078746,21.));
#17826=CARTESIAN_POINT('Ctrl Pts',(16.3217321000366,9.69000797146315,0.));
#17827=CARTESIAN_POINT('Ctrl Pts',(16.3217321000366,9.69000797146315,21.));
#17828=CARTESIAN_POINT('Ctrl Pts',(16.3579039682519,9.72060002001012,0.));
#17829=CARTESIAN_POINT('Ctrl Pts',(16.3579039682519,9.72060002001012,21.));
#17830=CARTESIAN_POINT('Ctrl Pts',(16.3938231282759,9.75159288382684,0.));
#17831=CARTESIAN_POINT('Ctrl Pts',(16.3938231282759,9.75159288382684,21.));
#17832=CARTESIAN_POINT('Ctrl Pts',(16.4295725710378,9.78285689698057,0.));
#17833=CARTESIAN_POINT('Ctrl Pts',(16.4295725710378,9.78285689698057,21.));
#17834=CARTESIAN_POINT('Ctrl Pts',(16.4651416449558,9.81439757053278,0.));
#17835=CARTESIAN_POINT('Ctrl Pts',(16.4651416449558,9.81439757053278,21.));
#17836=CARTESIAN_POINT('Ctrl Pts',(16.5004633692332,9.84630229363521,0.));
#17837=CARTESIAN_POINT('Ctrl Pts',(16.5004633692332,9.84630229363521,21.));
#17838=CARTESIAN_POINT('Ctrl Pts',(16.5354535643506,9.8786843754698,0.));
#17839=CARTESIAN_POINT('Ctrl Pts',(16.5354535643506,9.8786843754698,21.));
#17840=CARTESIAN_POINT('Ctrl Pts',(16.5700527532381,9.91162317616648,0.));
#17841=CARTESIAN_POINT('Ctrl Pts',(16.5700527532381,9.91162317616648,21.));
#17842=CARTESIAN_POINT('Ctrl Pts',(16.6042559779574,9.9451214271291,0.));
#17843=CARTESIAN_POINT('Ctrl Pts',(16.6042559779574,9.9451214271291,21.));
#17844=CARTESIAN_POINT('Ctrl Pts',(16.6380914029057,9.97913546489641,0.));
#17845=CARTESIAN_POINT('Ctrl Pts',(16.6380914029057,9.97913546489641,21.));
#17846=CARTESIAN_POINT('Ctrl Pts',(16.6716062376277,10.0135950379525,0.));
#17847=CARTESIAN_POINT('Ctrl Pts',(16.6716062376277,10.0135950379525,21.));
#17848=CARTESIAN_POINT('Ctrl Pts',(16.7048506904207,10.0484259314257,0.));
#17849=CARTESIAN_POINT('Ctrl Pts',(16.7048506904207,10.0484259314257,21.));
#17850=CARTESIAN_POINT('Ctrl Pts',(16.7378607357337,10.0835742491038,0.));
#17851=CARTESIAN_POINT('Ctrl Pts',(16.7378607357337,10.0835742491038,21.));
#17852=CARTESIAN_POINT('Ctrl Pts',(16.7706479198888,10.1190207721353,0.));
#17853=CARTESIAN_POINT('Ctrl Pts',(16.7706479198888,10.1190207721353,21.));
#17854=CARTESIAN_POINT('Ctrl Pts',(16.8032089941901,10.1547673397274,0.));
#17855=CARTESIAN_POINT('Ctrl Pts',(16.8032089941901,10.1547673397274,21.));
#17856=CARTESIAN_POINT('Ctrl Pts',(16.8355319435838,10.1908283166713,0.));
#17857=CARTESIAN_POINT('Ctrl Pts',(16.8355319435838,10.1908283166713,21.));
#17858=CARTESIAN_POINT('Ctrl Pts',(16.8676029947679,10.2272206796636,0.));
#17859=CARTESIAN_POINT('Ctrl Pts',(16.8676029947679,10.2272206796636,21.));
#17860=CARTESIAN_POINT('Ctrl Pts',(16.8994142530447,10.2639532144219,0.));
#17861=CARTESIAN_POINT('Ctrl Pts',(16.8994142530447,10.2639532144219,21.));
#17862=CARTESIAN_POINT('Ctrl Pts',(16.9309675442426,10.3010210756062,0.));
#17863=CARTESIAN_POINT('Ctrl Pts',(16.9309675442426,10.3010210756062,21.));
#17864=CARTESIAN_POINT('Ctrl Pts',(16.9622702798438,10.3384116178624,0.));
#17865=CARTESIAN_POINT('Ctrl Pts',(16.9622702798438,10.3384116178624,21.));
#17866=CARTESIAN_POINT('Ctrl Pts',(16.9933329788855,10.3761078860454,0.));
#17867=CARTESIAN_POINT('Ctrl Pts',(16.9933329788855,10.3761078860454,21.));
#17868=CARTESIAN_POINT('Ctrl Pts',(17.0241663361802,10.4140927470882,0.));
#17869=CARTESIAN_POINT('Ctrl Pts',(17.0241663361802,10.4140927470882,21.));
#17870=CARTESIAN_POINT('Ctrl Pts',(17.0547779975888,10.452353435089,0.));
#17871=CARTESIAN_POINT('Ctrl Pts',(17.0547779975888,10.452353435089,21.));
#17872=CARTESIAN_POINT('Ctrl Pts',(17.0851711712016,10.4908835057575,0.));
#17873=CARTESIAN_POINT('Ctrl Pts',(17.0851711712016,10.4908835057575,21.));
#17874=CARTESIAN_POINT('Ctrl Pts',(17.1153464189932,10.5296803023445,0.));
#17875=CARTESIAN_POINT('Ctrl Pts',(17.1153464189932,10.5296803023445,21.));
#17876=CARTESIAN_POINT('Ctrl Pts',(17.1453027387554,10.5687434234512,0.));
#17877=CARTESIAN_POINT('Ctrl Pts',(17.1453027387554,10.5687434234512,21.));
#17878=CARTESIAN_POINT('Ctrl Pts',(17.1750388395657,10.6080729180997,0.));
#17879=CARTESIAN_POINT('Ctrl Pts',(17.1750388395657,10.6080729180997,21.));
#17880=CARTESIAN_POINT('Ctrl Pts',(17.2045545572011,10.6476672831754,0.));
#17881=CARTESIAN_POINT('Ctrl Pts',(17.2045545572011,10.6476672831754,21.));
#17882=CARTESIAN_POINT('Ctrl Pts',(17.2338514174708,10.6875226650217,0.));
#17883=CARTESIAN_POINT('Ctrl Pts',(17.2338514174708,10.6875226650217,21.));
#17884=CARTESIAN_POINT('Ctrl Pts',(17.2629318816279,10.7276339231608,0.));
#17885=CARTESIAN_POINT('Ctrl Pts',(17.2629318816279,10.7276339231608,21.));
#17886=CARTESIAN_POINT('Ctrl Pts',(17.2917988998581,10.7679952591482,0.));
#17887=CARTESIAN_POINT('Ctrl Pts',(17.2917988998581,10.7679952591482,21.));
#17888=CARTESIAN_POINT('Ctrl Pts',(17.3204553814537,10.8086009632423,0.));
#17889=CARTESIAN_POINT('Ctrl Pts',(17.3204553814537,10.8086009632423,21.));
#17890=CARTESIAN_POINT('Ctrl Pts',(17.3489036079991,10.8494462423128,0.));
#17891=CARTESIAN_POINT('Ctrl Pts',(17.3489036079991,10.8494462423128,21.));
#17892=CARTESIAN_POINT('Ctrl Pts',(17.377145012528,10.8905275295837,0.));
#17893=CARTESIAN_POINT('Ctrl Pts',(17.377145012528,10.8905275295837,21.));
#17894=CARTESIAN_POINT('Ctrl Pts',(17.4051805054129,10.9318420203801,0.));
#17895=CARTESIAN_POINT('Ctrl Pts',(17.4051805054129,10.9318420203801,21.));
#17896=CARTESIAN_POINT('Ctrl Pts',(17.4330106728622,10.9733873885115,0.));
#17897=CARTESIAN_POINT('Ctrl Pts',(17.4330106728622,10.9733873885115,21.));
#17898=CARTESIAN_POINT('Ctrl Pts',(17.460636011184,11.0151614525642,0.));
#17899=CARTESIAN_POINT('Ctrl Pts',(17.460636011184,11.0151614525642,21.));
#17900=CARTESIAN_POINT('Ctrl Pts',(17.4880571878157,11.0571618040371,0.));
#17901=CARTESIAN_POINT('Ctrl Pts',(17.4880571878157,11.0571618040371,21.));
#17902=CARTESIAN_POINT('Ctrl Pts',(17.5152751467292,11.0993856581394,0.));
#17903=CARTESIAN_POINT('Ctrl Pts',(17.5152751467292,11.0993856581394,21.));
#17904=CARTESIAN_POINT('Ctrl Pts',(17.5422909714139,11.1418300507683,0.));
#17905=CARTESIAN_POINT('Ctrl Pts',(17.5422909714139,11.1418300507683,21.));
#17906=CARTESIAN_POINT('Ctrl Pts',(17.5691058058227,11.1844919535058,0.));
#17907=CARTESIAN_POINT('Ctrl Pts',(17.5691058058227,11.1844919535058,21.));
#17908=CARTESIAN_POINT('Ctrl Pts',(17.5957207597803,11.2273684103051,0.));
#17909=CARTESIAN_POINT('Ctrl Pts',(17.5957207597803,11.2273684103051,21.));
#17910=CARTESIAN_POINT('Ctrl Pts',(17.6221368072528,11.2704566868205,0.));
#17911=CARTESIAN_POINT('Ctrl Pts',(17.6221368072528,11.2704566868205,21.));
#17912=CARTESIAN_POINT('Ctrl Pts',(17.6483547422688,11.3137543310722,0.));
#17913=CARTESIAN_POINT('Ctrl Pts',(17.6483547422688,11.3137543310722,21.));
#17914=CARTESIAN_POINT('Ctrl Pts',(17.674375235974,11.3572590796967,0.));
#17915=CARTESIAN_POINT('Ctrl Pts',(17.674375235974,11.3572590796967,21.));
#17916=CARTESIAN_POINT('Ctrl Pts',(17.700198872213,11.4009687970126,0.));
#17917=CARTESIAN_POINT('Ctrl Pts',(17.700198872213,11.4009687970126,21.));
#17918=CARTESIAN_POINT('Ctrl Pts',(17.725826190457,11.4448814046804,0.));
#17919=CARTESIAN_POINT('Ctrl Pts',(17.725826190457,11.4448814046804,21.));
#17920=CARTESIAN_POINT('Ctrl Pts',(17.7512577332768,11.4889948016216,0.));
#17921=CARTESIAN_POINT('Ctrl Pts',(17.7512577332768,11.4889948016216,21.));
#17922=CARTESIAN_POINT('Ctrl Pts',(17.7764940721306,11.5333068279911,0.));
#17923=CARTESIAN_POINT('Ctrl Pts',(17.7764940721306,11.5333068279911,21.));
#17924=CARTESIAN_POINT('Ctrl Pts',(17.8015357852426,11.5778153222435,0.));
#17925=CARTESIAN_POINT('Ctrl Pts',(17.8015357852426,11.5778153222435,21.));
#17926=CARTESIAN_POINT('Ctrl Pts',(17.8263834470057,11.6225181583564,0.));
#17927=CARTESIAN_POINT('Ctrl Pts',(17.8263834470057,11.6225181583564,21.));
#17928=CARTESIAN_POINT('Ctrl Pts',(17.8510376144926,11.6674132861792,0.));
#17929=CARTESIAN_POINT('Ctrl Pts',(17.8510376144926,11.6674132861792,21.));
#17930=CARTESIAN_POINT('Ctrl Pts',(17.8754988158862,11.7124987772363,0.));
#17931=CARTESIAN_POINT('Ctrl Pts',(17.8754988158862,11.7124987772363,21.));
#17932=CARTESIAN_POINT('Ctrl Pts',(17.8997675418752,11.7577728408871,0.));
#17933=CARTESIAN_POINT('Ctrl Pts',(17.8997675418752,11.7577728408871,21.));
#17934=CARTESIAN_POINT('Ctrl Pts',(17.9238442458356,11.8032337607271,0.));
#17935=CARTESIAN_POINT('Ctrl Pts',(17.9238442458356,11.8032337607271,21.));
#17936=CARTESIAN_POINT('Ctrl Pts',(17.9477293432951,11.8488798430201,0.));
#17937=CARTESIAN_POINT('Ctrl Pts',(17.9477293432951,11.8488798430201,21.));
#17938=CARTESIAN_POINT('Ctrl Pts',(17.9714232133203,11.8947093631895,0.));
#17939=CARTESIAN_POINT('Ctrl Pts',(17.9714232133203,11.8947093631895,21.));
#17940=CARTESIAN_POINT('Ctrl Pts',(17.9949261997754,11.9407205019619,0.));
#17941=CARTESIAN_POINT('Ctrl Pts',(17.9949261997754,11.9407205019619,21.));
#17942=CARTESIAN_POINT('Ctrl Pts',(18.0182386160553,11.986911314246,0.));
#17943=CARTESIAN_POINT('Ctrl Pts',(18.0182386160553,11.986911314246,21.));
#17944=CARTESIAN_POINT('Ctrl Pts',(18.0413607600052,12.0332798395991,0.));
#17945=CARTESIAN_POINT('Ctrl Pts',(18.0413607600052,12.0332798395991,21.));
#17946=CARTESIAN_POINT('Ctrl Pts',(18.0642929289333,12.0798241915081,0.));
#17947=CARTESIAN_POINT('Ctrl Pts',(18.0642929289333,12.0798241915081,21.));
#17948=CARTESIAN_POINT('Ctrl Pts',(18.0870354350128,12.1265426519718,0.));
#17949=CARTESIAN_POINT('Ctrl Pts',(18.0870354350128,12.1265426519718,21.));
#17950=CARTESIAN_POINT('Ctrl Pts',(18.109588624154,12.1734337668195,0.));
#17951=CARTESIAN_POINT('Ctrl Pts',(18.109588624154,12.1734337668195,21.));
#17952=CARTESIAN_POINT('Ctrl Pts',(18.1319528884305,12.2204964278426,0.));
#17953=CARTESIAN_POINT('Ctrl Pts',(18.1319528884305,12.2204964278426,21.));
#17954=CARTESIAN_POINT('Ctrl Pts',(18.1541286139166,12.2677298318549,0.));
#17955=CARTESIAN_POINT('Ctrl Pts',(18.1541286139166,12.2677298318549,21.));
#17956=CARTESIAN_POINT('Ctrl Pts',(18.1717186310224,12.3056527265146,0.));
#17957=CARTESIAN_POINT('Ctrl Pts',(18.1717186310224,12.3056527265146,21.));
#17958=CARTESIAN_POINT('Ctrl Pts',(18.1848265584754,12.3341713636489,0.));
#17959=CARTESIAN_POINT('Ctrl Pts',(18.1848265584754,12.3341713636489,21.));
#17960=CARTESIAN_POINT('Ctrl Pts',(18.1935275957711,12.3532177620787,0.));
#17961=CARTESIAN_POINT('Ctrl Pts',(18.1935275957711,12.3532177620787,21.));
#17962=CARTESIAN_POINT('Ctrl Pts',(18.1978687191668,12.3627494547115,0.));
#17963=CARTESIAN_POINT('Ctrl Pts',(18.1978687191668,12.3627494547115,21.));
#17964=CARTESIAN_POINT('Ctrl Pts',(16.1689656784104,9.57984538049455,0.));
#17965=CARTESIAN_POINT('Ctrl Pts',(16.1770747160769,9.58464985151482,0.));
#17966=CARTESIAN_POINT('Ctrl Pts',(16.1931534965272,9.59446643316596,0.));
#17967=CARTESIAN_POINT('Ctrl Pts',(16.2168537871666,9.60981421781524,0.));
#17968=CARTESIAN_POINT('Ctrl Pts',(16.2476599387841,9.63146315443273,0.));
#17969=CARTESIAN_POINT('Ctrl Pts',(16.2850845948324,9.66014786078746,0.));
#17970=CARTESIAN_POINT('Ctrl Pts',(16.3217321000366,9.69000797146315,0.));
#17971=CARTESIAN_POINT('Ctrl Pts',(16.3579039682519,9.72060002001012,0.));
#17972=CARTESIAN_POINT('Ctrl Pts',(16.3938231282759,9.75159288382684,0.));
#17973=CARTESIAN_POINT('Ctrl Pts',(16.4295725710378,9.78285689698057,0.));
#17974=CARTESIAN_POINT('Ctrl Pts',(16.4651416449558,9.81439757053278,0.));
#17975=CARTESIAN_POINT('Ctrl Pts',(16.5004633692332,9.84630229363521,0.));
#17976=CARTESIAN_POINT('Ctrl Pts',(16.5354535643506,9.8786843754698,0.));
#17977=CARTESIAN_POINT('Ctrl Pts',(16.5700527532381,9.91162317616648,0.));
#17978=CARTESIAN_POINT('Ctrl Pts',(16.6042559779574,9.9451214271291,0.));
#17979=CARTESIAN_POINT('Ctrl Pts',(16.6380914029057,9.97913546489641,0.));
#17980=CARTESIAN_POINT('Ctrl Pts',(16.6716062376277,10.0135950379525,0.));
#17981=CARTESIAN_POINT('Ctrl Pts',(16.7048506904207,10.0484259314257,0.));
#17982=CARTESIAN_POINT('Ctrl Pts',(16.7378607357337,10.0835742491038,0.));
#17983=CARTESIAN_POINT('Ctrl Pts',(16.7706479198888,10.1190207721353,0.));
#17984=CARTESIAN_POINT('Ctrl Pts',(16.8032089941901,10.1547673397274,0.));
#17985=CARTESIAN_POINT('Ctrl Pts',(16.8355319435838,10.1908283166713,0.));
#17986=CARTESIAN_POINT('Ctrl Pts',(16.8676029947679,10.2272206796636,0.));
#17987=CARTESIAN_POINT('Ctrl Pts',(16.8994142530447,10.2639532144219,0.));
#17988=CARTESIAN_POINT('Ctrl Pts',(16.9309675442426,10.3010210756062,0.));
#17989=CARTESIAN_POINT('Ctrl Pts',(16.9622702798438,10.3384116178624,0.));
#17990=CARTESIAN_POINT('Ctrl Pts',(16.9933329788855,10.3761078860454,0.));
#17991=CARTESIAN_POINT('Ctrl Pts',(17.0241663361802,10.4140927470882,0.));
#17992=CARTESIAN_POINT('Ctrl Pts',(17.0547779975888,10.452353435089,0.));
#17993=CARTESIAN_POINT('Ctrl Pts',(17.0851711712016,10.4908835057575,0.));
#17994=CARTESIAN_POINT('Ctrl Pts',(17.1153464189932,10.5296803023445,0.));
#17995=CARTESIAN_POINT('Ctrl Pts',(17.1453027387554,10.5687434234512,0.));
#17996=CARTESIAN_POINT('Ctrl Pts',(17.1750388395657,10.6080729180997,0.));
#17997=CARTESIAN_POINT('Ctrl Pts',(17.2045545572011,10.6476672831754,0.));
#17998=CARTESIAN_POINT('Ctrl Pts',(17.2338514174708,10.6875226650217,0.));
#17999=CARTESIAN_POINT('Ctrl Pts',(17.2629318816279,10.7276339231608,0.));
#18000=CARTESIAN_POINT('Ctrl Pts',(17.2917988998581,10.7679952591482,0.));
#18001=CARTESIAN_POINT('Ctrl Pts',(17.3204553814537,10.8086009632423,0.));
#18002=CARTESIAN_POINT('Ctrl Pts',(17.3489036079991,10.8494462423128,0.));
#18003=CARTESIAN_POINT('Ctrl Pts',(17.377145012528,10.8905275295837,0.));
#18004=CARTESIAN_POINT('Ctrl Pts',(17.4051805054129,10.9318420203801,0.));
#18005=CARTESIAN_POINT('Ctrl Pts',(17.4330106728622,10.9733873885115,0.));
#18006=CARTESIAN_POINT('Ctrl Pts',(17.460636011184,11.0151614525642,0.));
#18007=CARTESIAN_POINT('Ctrl Pts',(17.4880571878157,11.0571618040371,0.));
#18008=CARTESIAN_POINT('Ctrl Pts',(17.5152751467292,11.0993856581394,0.));
#18009=CARTESIAN_POINT('Ctrl Pts',(17.5422909714139,11.1418300507683,0.));
#18010=CARTESIAN_POINT('Ctrl Pts',(17.5691058058227,11.1844919535058,0.));
#18011=CARTESIAN_POINT('Ctrl Pts',(17.5957207597803,11.2273684103051,0.));
#18012=CARTESIAN_POINT('Ctrl Pts',(17.6221368072528,11.2704566868205,0.));
#18013=CARTESIAN_POINT('Ctrl Pts',(17.6483547422688,11.3137543310722,0.));
#18014=CARTESIAN_POINT('Ctrl Pts',(17.674375235974,11.3572590796967,0.));
#18015=CARTESIAN_POINT('Ctrl Pts',(17.700198872213,11.4009687970126,0.));
#18016=CARTESIAN_POINT('Ctrl Pts',(17.725826190457,11.4448814046804,0.));
#18017=CARTESIAN_POINT('Ctrl Pts',(17.7512577332768,11.4889948016216,0.));
#18018=CARTESIAN_POINT('Ctrl Pts',(17.7764940721306,11.5333068279911,0.));
#18019=CARTESIAN_POINT('Ctrl Pts',(17.8015357852426,11.5778153222435,0.));
#18020=CARTESIAN_POINT('Ctrl Pts',(17.8263834470057,11.6225181583564,0.));
#18021=CARTESIAN_POINT('Ctrl Pts',(17.8510376144926,11.6674132861792,0.));
#18022=CARTESIAN_POINT('Ctrl Pts',(17.8754988158862,11.7124987772363,0.));
#18023=CARTESIAN_POINT('Ctrl Pts',(17.8997675418752,11.7577728408871,0.));
#18024=CARTESIAN_POINT('Ctrl Pts',(17.9238442458356,11.8032337607271,0.));
#18025=CARTESIAN_POINT('Ctrl Pts',(17.9477293432951,11.8488798430201,0.));
#18026=CARTESIAN_POINT('Ctrl Pts',(17.9714232133203,11.8947093631895,0.));
#18027=CARTESIAN_POINT('Ctrl Pts',(17.9949261997754,11.9407205019619,0.));
#18028=CARTESIAN_POINT('Ctrl Pts',(18.0182386160553,11.986911314246,0.));
#18029=CARTESIAN_POINT('Ctrl Pts',(18.0413607600052,12.0332798395991,0.));
#18030=CARTESIAN_POINT('Ctrl Pts',(18.0642929289333,12.0798241915081,0.));
#18031=CARTESIAN_POINT('Ctrl Pts',(18.0870354350128,12.1265426519718,0.));
#18032=CARTESIAN_POINT('Ctrl Pts',(18.109588624154,12.1734337668195,0.));
#18033=CARTESIAN_POINT('Ctrl Pts',(18.1364257412858,12.2299089600472,0.));
#18034=CARTESIAN_POINT('Ctrl Pts',(18.1585543320743,12.2771850498068,0.));
#18035=CARTESIAN_POINT('Ctrl Pts',(18.1761067306718,12.3151419520839,0.));
#18036=CARTESIAN_POINT('Ctrl Pts',(18.1891864723772,12.3436860694314,0.));
#18037=CARTESIAN_POINT('Ctrl Pts',(18.1978687191668,12.3627494547115,0.));
#18038=CARTESIAN_POINT('Ctrl Pts',(16.1689656784104,9.57984538049455,13.));
#18039=CARTESIAN_POINT('Ctrl Pts',(16.1826331205334,9.58794311444298,13.));
#18040=CARTESIAN_POINT('Ctrl Pts',(16.1960605405031,9.59639855902712,13.));
#18041=CARTESIAN_POINT('Ctrl Pts',(16.209264165571,9.60518801711085,13.));
#18042=CARTESIAN_POINT('Ctrl Pts',(16.224739801703,9.6154899193841,13.));
#18043=CARTESIAN_POINT('Ctrl Pts',(16.2399084848584,9.62624998107167,13.));
#18044=CARTESIAN_POINT('Ctrl Pts',(16.254836637175,9.63737105568732,13.));
#18045=CARTESIAN_POINT('Ctrl Pts',(16.2758412618972,9.65301893989003,13.));
#18046=CARTESIAN_POINT('Ctrl Pts',(16.296373798599,9.66937567449949,13.));
#18047=CARTESIAN_POINT('Ctrl Pts',(16.3166650331518,9.68610238201322,13.));
#18048=CARTESIAN_POINT('Ctrl Pts',(16.3301619042985,9.69722828051063,13.));
#18049=CARTESIAN_POINT('Ctrl Pts',(16.3435531467518,9.70851618070807,13.));
#18050=CARTESIAN_POINT('Ctrl Pts',(16.3568892752788,9.7198910779208,13.));
#18051=CARTESIAN_POINT('Ctrl Pts',(16.3709277366574,9.73186502184932,13.));
#18052=CARTESIAN_POINT('Ctrl Pts',(16.3849056240572,9.74393463776872,13.));
#18053=CARTESIAN_POINT('Ctrl Pts',(16.3988451548219,9.75606525513648,13.));
#18054=CARTESIAN_POINT('Ctrl Pts',(16.414325766791,9.76953696975778,13.));
#18055=CARTESIAN_POINT('Ctrl Pts',(16.4297583183324,9.78308498747417,13.));
#18056=CARTESIAN_POINT('Ctrl Pts',(16.4451338763398,9.79671869019648,13.));
#18057=CARTESIAN_POINT('Ctrl Pts',(16.4683132763075,9.8172721587789,13.));
#18058=CARTESIAN_POINT('Ctrl Pts',(16.4913594464712,9.83802550134249,13.));
#18059=CARTESIAN_POINT('Ctrl Pts',(16.5141788054336,9.8591036086492,13.));
#18060=CARTESIAN_POINT('Ctrl Pts',(16.5307565708362,9.87441639279171,13.));
#18061=CARTESIAN_POINT('Ctrl Pts',(16.5472127770975,9.88990330206224,13.));
#18062=CARTESIAN_POINT('Ctrl Pts',(16.5635345032205,9.90558047214324,13.));
#18063=CARTESIAN_POINT('Ctrl Pts',(16.5834864158081,9.92474447016174,13.));
#18064=CARTESIAN_POINT('Ctrl Pts',(16.6032381063718,9.94419173110009,13.));
#18065=CARTESIAN_POINT('Ctrl Pts',(16.6228156007807,9.96388214930655,13.));
#18066=CARTESIAN_POINT('Ctrl Pts',(16.6439625439398,9.9851510689085,13.));
#18067=CARTESIAN_POINT('Ctrl Pts',(16.6649096998191,10.006698815053,13.));
#18068=CARTESIAN_POINT('Ctrl Pts',(16.6857083247995,10.0284493480904,13.));
#18069=CARTESIAN_POINT('Ctrl Pts',(16.7049095176705,10.0485293380076,13.));
#18070=CARTESIAN_POINT('Ctrl Pts',(16.7239855768682,10.0687801145851,13.));
#18071=CARTESIAN_POINT('Ctrl Pts',(16.7429517500628,10.0891775910162,13.));
#18072=CARTESIAN_POINT('Ctrl Pts',(16.7687182701337,10.1168886100216,13.));
#18073=CARTESIAN_POINT('Ctrl Pts',(16.7942808297111,10.1448719871919,13.));
#18074=CARTESIAN_POINT('Ctrl Pts',(16.8196194580035,10.1731502199822,13.));
#18075=CARTESIAN_POINT('Ctrl Pts',(16.8440706870575,10.200438103889,13.));
#18076=CARTESIAN_POINT('Ctrl Pts',(16.8683088890845,10.22800693093,13.));
#18077=CARTESIAN_POINT('Ctrl Pts',(16.8923226175348,10.2558682820695,13.));
#18078=CARTESIAN_POINT('Ctrl Pts',(16.9249459403077,10.2937187080453,13.));
#18079=CARTESIAN_POINT('Ctrl Pts',(16.957156835636,10.3321063567987,13.));
#18080=CARTESIAN_POINT('Ctrl Pts',(16.9889999235631,10.3709578724441,13.));
#18081=CARTESIAN_POINT('Ctrl Pts',(17.0169893056038,10.4051075100907,13.));
#18082=CARTESIAN_POINT('Ctrl Pts',(17.0446984863548,10.4396099589581,13.));
#18083=CARTESIAN_POINT('Ctrl Pts',(17.0721430002005,10.4744368762492,13.));
#18084=CARTESIAN_POINT('Ctrl Pts',(17.112602877038,10.5257802081858,13.));
#18085=CARTESIAN_POINT('Ctrl Pts',(17.1524822680213,10.5778361036166,13.));
#18086=CARTESIAN_POINT('Ctrl Pts',(17.1917748564439,10.6305946314109,13.));
#18087=CARTESIAN_POINT('Ctrl Pts',(17.2413624862159,10.6971764079904,13.));
#18088=CARTESIAN_POINT('Ctrl Pts',(17.2900185097256,10.7648729796203,13.));
#18089=CARTESIAN_POINT('Ctrl Pts',(17.3377983049414,10.8335716332062,13.));
#18090=CARTESIAN_POINT('Ctrl Pts',(17.4025197210759,10.9266292557124,13.));
#18091=CARTESIAN_POINT('Ctrl Pts',(17.465629946413,11.0215303642373,13.));
#18092=CARTESIAN_POINT('Ctrl Pts',(17.5271690583425,11.1181400554142,13.));
#18093=CARTESIAN_POINT('Ctrl Pts',(17.5820327884924,11.2042701255502,13.));
#18094=CARTESIAN_POINT('Ctrl Pts',(17.6356526662298,11.2917512652669,13.));
#18095=CARTESIAN_POINT('Ctrl Pts',(17.6880597469793,11.3804891386312,13.));
#18096=CARTESIAN_POINT('Ctrl Pts',(17.7623349917745,11.5062551071316,13.));
#18097=CARTESIAN_POINT('Ctrl Pts',(17.8341701535693,11.6345494475267,13.));
#18098=CARTESIAN_POINT('Ctrl Pts',(17.9036238122721,11.7651542351076,13.));
#18099=CARTESIAN_POINT('Ctrl Pts',(17.9575737615817,11.8666049261321,13.));
#18100=CARTESIAN_POINT('Ctrl Pts',(18.0100864746848,11.9694546915729,13.));
#18101=CARTESIAN_POINT('Ctrl Pts',(18.0611784501166,12.0736101882024,13.));
#18102=CARTESIAN_POINT('Ctrl Pts',(18.105376864951,12.1637125537578,13.));
#18103=CARTESIAN_POINT('Ctrl Pts',(18.148512095574,12.2547877896022,13.));
#18104=CARTESIAN_POINT('Ctrl Pts',(18.1905949538311,12.3468112455713,13.));
#18105=CARTESIAN_POINT('Ctrl Pts',(18.193023049118,12.3521208117218,13.));
#18106=CARTESIAN_POINT('Ctrl Pts',(18.1954476374996,12.3574335481621,13.));
#18107=CARTESIAN_POINT('Ctrl Pts',(18.1978687191668,12.3627494547115,13.));
#18108=CARTESIAN_POINT('Ctrl Pts',(20.698113262342,7.45574324794401,0.));
#18109=CARTESIAN_POINT('Ctrl Pts',(20.698113262342,7.45574324794401,21.));
#18110=CARTESIAN_POINT('Ctrl Pts',(20.6878503127065,7.45783379370107,0.));
#18111=CARTESIAN_POINT('Ctrl Pts',(20.6878503127065,7.45783379370107,21.));
#18112=CARTESIAN_POINT('Ctrl Pts',(20.6673271112931,7.46198969876653,0.));
#18113=CARTESIAN_POINT('Ctrl Pts',(20.6673271112931,7.46198969876653,21.));
#18114=CARTESIAN_POINT('Ctrl Pts',(20.6365504027501,7.46814799701905,0.));
#18115=CARTESIAN_POINT('Ctrl Pts',(20.6365504027501,7.46814799701905,21.));
#18116=CARTESIAN_POINT('Ctrl Pts',(20.5955309838521,7.47620789245428,0.));
#18117=CARTESIAN_POINT('Ctrl Pts',(20.5955309838521,7.47620789245428,21.));
#18118=CARTESIAN_POINT('Ctrl Pts',(20.5442837929044,7.48603045196744,0.));
#18119=CARTESIAN_POINT('Ctrl Pts',(20.5442837929044,7.48603045196744,21.));
#18120=CARTESIAN_POINT('Ctrl Pts',(20.4930639156161,7.49560012018405,0.));
#18121=CARTESIAN_POINT('Ctrl Pts',(20.4930639156161,7.49560012018405,21.));
#18122=CARTESIAN_POINT('Ctrl Pts',(20.4418717748497,7.50491611266253,0.));
#18123=CARTESIAN_POINT('Ctrl Pts',(20.4418717748497,7.50491611266253,21.));
#18124=CARTESIAN_POINT('Ctrl Pts',(20.3907080367098,7.51397746081993,0.));
#18125=CARTESIAN_POINT('Ctrl Pts',(20.3907080367098,7.51397746081993,21.));
#18126=CARTESIAN_POINT('Ctrl Pts',(20.3395736743243,7.52278303006887,0.));
#18127=CARTESIAN_POINT('Ctrl Pts',(20.3395736743243,7.52278303006887,21.));
#18128=CARTESIAN_POINT('Ctrl Pts',(20.2884698940944,7.53133155804008,0.));
#18129=CARTESIAN_POINT('Ctrl Pts',(20.2884698940944,7.53133155804008,21.));
#18130=CARTESIAN_POINT('Ctrl Pts',(20.2373980474879,7.53962169534167,0.));
#18131=CARTESIAN_POINT('Ctrl Pts',(20.2373980474879,7.53962169534167,21.));
#18132=CARTESIAN_POINT('Ctrl Pts',(20.1863595454674,7.54765204869254,0.));
#18133=CARTESIAN_POINT('Ctrl Pts',(20.1863595454674,7.54765204869254,21.));
#18134=CARTESIAN_POINT('Ctrl Pts',(20.1353557774357,7.55542122125494,0.));
#18135=CARTESIAN_POINT('Ctrl Pts',(20.1353557774357,7.55542122125494,21.));
#18136=CARTESIAN_POINT('Ctrl Pts',(20.0843880130978,7.5629278654946,0.));
#18137=CARTESIAN_POINT('Ctrl Pts',(20.0843880130978,7.5629278654946,21.));
#18138=CARTESIAN_POINT('Ctrl Pts',(20.0334574248556,7.57017066105973,0.));
#18139=CARTESIAN_POINT('Ctrl Pts',(20.0334574248556,7.57017066105973,21.));
#18140=CARTESIAN_POINT('Ctrl Pts',(19.9825651387294,7.57714827622806,0.));
#18141=CARTESIAN_POINT('Ctrl Pts',(19.9825651387294,7.57714827622806,21.));
#18142=CARTESIAN_POINT('Ctrl Pts',(19.931712276832,7.58385933533351,0.));
#18143=CARTESIAN_POINT('Ctrl Pts',(19.931712276832,7.58385933533351,21.));
#18144=CARTESIAN_POINT('Ctrl Pts',(19.8808999994024,7.59030238888852,0.));
#18145=CARTESIAN_POINT('Ctrl Pts',(19.8808999994024,7.59030238888852,21.));
#18146=CARTESIAN_POINT('Ctrl Pts',(19.830129556152,7.59647587605448,0.));
#18147=CARTESIAN_POINT('Ctrl Pts',(19.830129556152,7.59647587605448,21.));
#18148=CARTESIAN_POINT('Ctrl Pts',(19.7794022782484,7.60237814110186,0.));
#18149=CARTESIAN_POINT('Ctrl Pts',(19.7794022782484,7.60237814110186,21.));
#18150=CARTESIAN_POINT('Ctrl Pts',(19.7287195480601,7.60800746969261,0.));
#18151=CARTESIAN_POINT('Ctrl Pts',(19.7287195480601,7.60800746969261,21.));
#18152=CARTESIAN_POINT('Ctrl Pts',(19.6780827744426,7.61336212350879,0.));
#18153=CARTESIAN_POINT('Ctrl Pts',(19.6780827744426,7.61336212350879,21.));
#18154=CARTESIAN_POINT('Ctrl Pts',(19.6274933688524,7.6184403707059,0.));
#18155=CARTESIAN_POINT('Ctrl Pts',(19.6274933688524,7.6184403707059,21.));
#18156=CARTESIAN_POINT('Ctrl Pts',(19.5769527121826,7.62324053735219,0.));
#18157=CARTESIAN_POINT('Ctrl Pts',(19.5769527121826,7.62324053735219,21.));
#18158=CARTESIAN_POINT('Ctrl Pts',(19.5264621687521,7.62776096538883,0.));
#18159=CARTESIAN_POINT('Ctrl Pts',(19.5264621687521,7.62776096538883,21.));
#18160=CARTESIAN_POINT('Ctrl Pts',(19.4760231231881,7.63199992715365,0.));
#18161=CARTESIAN_POINT('Ctrl Pts',(19.4760231231881,7.63199992715365,21.));
#18162=CARTESIAN_POINT('Ctrl Pts',(19.4256370121006,7.63595554930654,0.));
#18163=CARTESIAN_POINT('Ctrl Pts',(19.4256370121006,7.63595554930654,21.));
#18164=CARTESIAN_POINT('Ctrl Pts',(19.3753053524647,7.6396257482276,0.));
#18165=CARTESIAN_POINT('Ctrl Pts',(19.3753053524647,7.6396257482276,21.));
#18166=CARTESIAN_POINT('Ctrl Pts',(19.3250297839295,7.64300812875339,0.));
#18167=CARTESIAN_POINT('Ctrl Pts',(19.3250297839295,7.64300812875339,21.));
#18168=CARTESIAN_POINT('Ctrl Pts',(19.2748120456486,7.64610005549613,0.));
#18169=CARTESIAN_POINT('Ctrl Pts',(19.2748120456486,7.64610005549613,21.));
#18170=CARTESIAN_POINT('Ctrl Pts',(19.224653915265,7.64889882291923,0.));
#18171=CARTESIAN_POINT('Ctrl Pts',(19.224653915265,7.64889882291923,21.));
#18172=CARTESIAN_POINT('Ctrl Pts',(19.1745571539291,7.65140181220525,0.));
#18173=CARTESIAN_POINT('Ctrl Pts',(19.1745571539291,7.65140181220525,21.));
#18174=CARTESIAN_POINT('Ctrl Pts',(19.1245234597312,7.65360662280609,0.));
#18175=CARTESIAN_POINT('Ctrl Pts',(19.1245234597312,7.65360662280609,21.));
#18176=CARTESIAN_POINT('Ctrl Pts',(19.0745543888799,7.65551129907201,0.));
#18177=CARTESIAN_POINT('Ctrl Pts',(19.0745543888799,7.65551129907201,21.));
#18178=CARTESIAN_POINT('Ctrl Pts',(19.0246514144531,7.65711415727855,0.));
#18179=CARTESIAN_POINT('Ctrl Pts',(19.0246514144531,7.65711415727855,21.));
#18180=CARTESIAN_POINT('Ctrl Pts',(18.974816073814,7.65841335587266,0.));
#18181=CARTESIAN_POINT('Ctrl Pts',(18.974816073814,7.65841335587266,21.));
#18182=CARTESIAN_POINT('Ctrl Pts',(18.9250501008887,7.65940650980099,0.));
#18183=CARTESIAN_POINT('Ctrl Pts',(18.9250501008887,7.65940650980099,21.));
#18184=CARTESIAN_POINT('Ctrl Pts',(18.8753555389435,7.66009036321663,0.));
#18185=CARTESIAN_POINT('Ctrl Pts',(18.8753555389435,7.66009036321663,21.));
#18186=CARTESIAN_POINT('Ctrl Pts',(18.8257349246207,7.66046025294775,0.));
#18187=CARTESIAN_POINT('Ctrl Pts',(18.8257349246207,7.66046025294775,21.));
#18188=CARTESIAN_POINT('Ctrl Pts',(18.7761911671591,7.6605104692254,0.));
#18189=CARTESIAN_POINT('Ctrl Pts',(18.7761911671591,7.6605104692254,21.));
#18190=CARTESIAN_POINT('Ctrl Pts',(18.7267272235231,7.66023521705904,0.));
#18191=CARTESIAN_POINT('Ctrl Pts',(18.7267272235231,7.66023521705904,21.));
#18192=CARTESIAN_POINT('Ctrl Pts',(18.6773458057584,7.65962948375621,0.));
#18193=CARTESIAN_POINT('Ctrl Pts',(18.6773458057584,7.65962948375621,21.));
#18194=CARTESIAN_POINT('Ctrl Pts',(18.6280491346907,7.65868976978872,0.));
#18195=CARTESIAN_POINT('Ctrl Pts',(18.6280491346907,7.65868976978872,21.));
#18196=CARTESIAN_POINT('Ctrl Pts',(18.5788385228928,7.65741532450727,0.));
#18197=CARTESIAN_POINT('Ctrl Pts',(18.5788385228928,7.65741532450727,21.));
#18198=CARTESIAN_POINT('Ctrl Pts',(18.5297146894905,7.65580722110437,0.));
#18199=CARTESIAN_POINT('Ctrl Pts',(18.5297146894905,7.65580722110437,21.));
#18200=CARTESIAN_POINT('Ctrl Pts',(18.4806785483052,7.65386603444743,0.));
#18201=CARTESIAN_POINT('Ctrl Pts',(18.4806785483052,7.65386603444743,21.));
#18202=CARTESIAN_POINT('Ctrl Pts',(18.4317319183719,7.65158974829126,0.));
#18203=CARTESIAN_POINT('Ctrl Pts',(18.4317319183719,7.65158974829126,21.));
#18204=CARTESIAN_POINT('Ctrl Pts',(18.3828781275628,7.6489719793775,0.));
#18205=CARTESIAN_POINT('Ctrl Pts',(18.3828781275628,7.6489719793775,21.));
#18206=CARTESIAN_POINT('Ctrl Pts',(18.3341230095852,7.64599903846601,0.));
#18207=CARTESIAN_POINT('Ctrl Pts',(18.3341230095852,7.64599903846601,21.));
#18208=CARTESIAN_POINT('Ctrl Pts',(18.2854741391282,7.6426522027076,0.));
#18209=CARTESIAN_POINT('Ctrl Pts',(18.2854741391282,7.6426522027076,21.));
#18210=CARTESIAN_POINT('Ctrl Pts',(18.2369390502576,7.63891299603826,0.));
#18211=CARTESIAN_POINT('Ctrl Pts',(18.2369390502576,7.63891299603826,21.));
#18212=CARTESIAN_POINT('Ctrl Pts',(18.1885236169197,7.63476798969016,0.));
#18213=CARTESIAN_POINT('Ctrl Pts',(18.1885236169197,7.63476798969016,21.));
#18214=CARTESIAN_POINT('Ctrl Pts',(18.1402306858819,7.63021285851761,0.));
#18215=CARTESIAN_POINT('Ctrl Pts',(18.1402306858819,7.63021285851761,21.));
#18216=CARTESIAN_POINT('Ctrl Pts',(18.0920577897363,7.62525915358073,0.));
#18217=CARTESIAN_POINT('Ctrl Pts',(18.0920577897363,7.62525915358073,21.));
#18218=CARTESIAN_POINT('Ctrl Pts',(18.0439992897906,7.61992799636654,0.));
#18219=CARTESIAN_POINT('Ctrl Pts',(18.0439992897906,7.61992799636654,21.));
#18220=CARTESIAN_POINT('Ctrl Pts',(17.9960506269561,7.61423755067037,0.));
#18221=CARTESIAN_POINT('Ctrl Pts',(17.9960506269561,7.61423755067037,21.));
#18222=CARTESIAN_POINT('Ctrl Pts',(17.9482122228183,7.60819152580111,0.));
#18223=CARTESIAN_POINT('Ctrl Pts',(17.9482122228183,7.60819152580111,21.));
#18224=CARTESIAN_POINT('Ctrl Pts',(17.900492838997,7.60176928403058,0.));
#18225=CARTESIAN_POINT('Ctrl Pts',(17.900492838997,7.60176928403058,21.));
#18226=CARTESIAN_POINT('Ctrl Pts',(17.8529149331931,7.59491004201955,0.));
#18227=CARTESIAN_POINT('Ctrl Pts',(17.8529149331931,7.59491004201955,21.));
#18228=CARTESIAN_POINT('Ctrl Pts',(17.8055090348024,7.58752955799499,0.));
#18229=CARTESIAN_POINT('Ctrl Pts',(17.8055090348024,7.58752955799499,21.));
#18230=CARTESIAN_POINT('Ctrl Pts',(17.7583042294209,7.57954834582803,0.));
#18231=CARTESIAN_POINT('Ctrl Pts',(17.7583042294209,7.57954834582803,21.));
#18232=CARTESIAN_POINT('Ctrl Pts',(17.7113192869136,7.57091795530423,0.));
#18233=CARTESIAN_POINT('Ctrl Pts',(17.7113192869136,7.57091795530423,21.));
#18234=CARTESIAN_POINT('Ctrl Pts',(17.6645549117314,7.56164400295863,0.));
#18235=CARTESIAN_POINT('Ctrl Pts',(17.6645549117314,7.56164400295863,21.));
#18236=CARTESIAN_POINT('Ctrl Pts',(17.6179818599248,7.55182125346563,0.));
#18237=CARTESIAN_POINT('Ctrl Pts',(17.6179818599248,7.55182125346563,21.));
#18238=CARTESIAN_POINT('Ctrl Pts',(17.5715579419204,7.54158441095317,0.));
#18239=CARTESIAN_POINT('Ctrl Pts',(17.5715579419204,7.54158441095317,21.));
#18240=CARTESIAN_POINT('Ctrl Pts',(17.5252518287336,7.53103903007863,0.));
#18241=CARTESIAN_POINT('Ctrl Pts',(17.5252518287336,7.53103903007863,21.));
#18242=CARTESIAN_POINT('Ctrl Pts',(17.4790653226646,7.52019696747328,0.));
#18243=CARTESIAN_POINT('Ctrl Pts',(17.4790653226646,7.52019696747328,21.));
#18244=CARTESIAN_POINT('Ctrl Pts',(17.4330545448126,7.50891486634214,0.));
#18245=CARTESIAN_POINT('Ctrl Pts',(17.4330545448126,7.50891486634214,21.));
#18246=CARTESIAN_POINT('Ctrl Pts',(17.3873563447297,7.49681774451751,0.));
#18247=CARTESIAN_POINT('Ctrl Pts',(17.3873563447297,7.49681774451751,21.));
#18248=CARTESIAN_POINT('Ctrl Pts',(17.3421522689127,7.48340100912745,0.));
#18249=CARTESIAN_POINT('Ctrl Pts',(17.3421522689127,7.48340100912745,21.));
#18250=CARTESIAN_POINT('Ctrl Pts',(17.3065305096784,7.47120323460919,0.));
#18251=CARTESIAN_POINT('Ctrl Pts',(17.3065305096784,7.47120323460919,21.));
#18252=CARTESIAN_POINT('Ctrl Pts',(17.2801832097582,7.4610504981825,0.));
#18253=CARTESIAN_POINT('Ctrl Pts',(17.2801832097582,7.4610504981825,21.));
#18254=CARTESIAN_POINT('Ctrl Pts',(17.2627905583523,7.45381253347183,0.));
#18255=CARTESIAN_POINT('Ctrl Pts',(17.2627905583523,7.45381253347183,21.));
#18256=CARTESIAN_POINT('Ctrl Pts',(17.2541372868972,7.45007618140238,0.));
#18257=CARTESIAN_POINT('Ctrl Pts',(17.2541372868972,7.45007618140238,21.));
#18258=CARTESIAN_POINT('',(20.698113262342,7.45574324794407,0.));
#18259=CARTESIAN_POINT('Ctrl Pts',(17.2541372868972,7.45007618140238,0.));
#18260=CARTESIAN_POINT('Ctrl Pts',(17.2627905583523,7.45381253347183,0.));
#18261=CARTESIAN_POINT('Ctrl Pts',(17.2801832097582,7.4610504981825,0.));
#18262=CARTESIAN_POINT('Ctrl Pts',(17.3065305096784,7.47120323460919,0.));
#18263=CARTESIAN_POINT('Ctrl Pts',(17.3421522689127,7.48340100912745,0.));
#18264=CARTESIAN_POINT('Ctrl Pts',(17.3873563447297,7.49681774451751,0.));
#18265=CARTESIAN_POINT('Ctrl Pts',(17.4330545448126,7.50891486634214,0.));
#18266=CARTESIAN_POINT('Ctrl Pts',(17.4790653226646,7.52019696747328,0.));
#18267=CARTESIAN_POINT('Ctrl Pts',(17.5252518287336,7.53103903007863,0.));
#18268=CARTESIAN_POINT('Ctrl Pts',(17.5715579419204,7.54158441095317,0.));
#18269=CARTESIAN_POINT('Ctrl Pts',(17.6179818599248,7.55182125346563,0.));
#18270=CARTESIAN_POINT('Ctrl Pts',(17.6645549117314,7.56164400295863,0.));
#18271=CARTESIAN_POINT('Ctrl Pts',(17.7113192869136,7.57091795530423,0.));
#18272=CARTESIAN_POINT('Ctrl Pts',(17.7583042294209,7.57954834582803,0.));
#18273=CARTESIAN_POINT('Ctrl Pts',(17.8055090348024,7.58752955799499,0.));
#18274=CARTESIAN_POINT('Ctrl Pts',(17.8529149331931,7.59491004201955,0.));
#18275=CARTESIAN_POINT('Ctrl Pts',(17.900492838997,7.60176928403058,0.));
#18276=CARTESIAN_POINT('Ctrl Pts',(17.9482122228183,7.60819152580111,0.));
#18277=CARTESIAN_POINT('Ctrl Pts',(17.9960506269561,7.61423755067037,0.));
#18278=CARTESIAN_POINT('Ctrl Pts',(18.0439992897906,7.61992799636654,0.));
#18279=CARTESIAN_POINT('Ctrl Pts',(18.0920577897363,7.62525915358073,0.));
#18280=CARTESIAN_POINT('Ctrl Pts',(18.1402306858819,7.63021285851761,0.));
#18281=CARTESIAN_POINT('Ctrl Pts',(18.1885236169197,7.63476798969016,0.));
#18282=CARTESIAN_POINT('Ctrl Pts',(18.2369390502576,7.63891299603826,0.));
#18283=CARTESIAN_POINT('Ctrl Pts',(18.2854741391282,7.6426522027076,0.));
#18284=CARTESIAN_POINT('Ctrl Pts',(18.3341230095852,7.64599903846601,0.));
#18285=CARTESIAN_POINT('Ctrl Pts',(18.3828781275628,7.6489719793775,0.));
#18286=CARTESIAN_POINT('Ctrl Pts',(18.4317319183719,7.65158974829126,0.));
#18287=CARTESIAN_POINT('Ctrl Pts',(18.4806785483052,7.65386603444743,0.));
#18288=CARTESIAN_POINT('Ctrl Pts',(18.5297146894905,7.65580722110437,0.));
#18289=CARTESIAN_POINT('Ctrl Pts',(18.5788385228928,7.65741532450727,0.));
#18290=CARTESIAN_POINT('Ctrl Pts',(18.6280491346907,7.65868976978872,0.));
#18291=CARTESIAN_POINT('Ctrl Pts',(18.6773458057584,7.65962948375621,0.));
#18292=CARTESIAN_POINT('Ctrl Pts',(18.7267272235231,7.66023521705904,0.));
#18293=CARTESIAN_POINT('Ctrl Pts',(18.7761911671591,7.6605104692254,0.));
#18294=CARTESIAN_POINT('Ctrl Pts',(18.8257349246207,7.66046025294775,0.));
#18295=CARTESIAN_POINT('Ctrl Pts',(18.8753555389435,7.66009036321663,0.));
#18296=CARTESIAN_POINT('Ctrl Pts',(18.9250501008887,7.65940650980099,0.));
#18297=CARTESIAN_POINT('Ctrl Pts',(18.974816073814,7.65841335587266,0.));
#18298=CARTESIAN_POINT('Ctrl Pts',(19.0246514144531,7.65711415727855,0.));
#18299=CARTESIAN_POINT('Ctrl Pts',(19.0745543888799,7.65551129907201,0.));
#18300=CARTESIAN_POINT('Ctrl Pts',(19.1245234597312,7.65360662280609,0.));
#18301=CARTESIAN_POINT('Ctrl Pts',(19.1745571539291,7.65140181220525,0.));
#18302=CARTESIAN_POINT('Ctrl Pts',(19.224653915265,7.64889882291923,0.));
#18303=CARTESIAN_POINT('Ctrl Pts',(19.2748120456486,7.64610005549613,0.));
#18304=CARTESIAN_POINT('Ctrl Pts',(19.3250297839295,7.64300812875339,0.));
#18305=CARTESIAN_POINT('Ctrl Pts',(19.3753053524647,7.6396257482276,0.));
#18306=CARTESIAN_POINT('Ctrl Pts',(19.4256370121006,7.63595554930654,0.));
#18307=CARTESIAN_POINT('Ctrl Pts',(19.4760231231881,7.63199992715365,0.));
#18308=CARTESIAN_POINT('Ctrl Pts',(19.5264621687521,7.62776096538883,0.));
#18309=CARTESIAN_POINT('Ctrl Pts',(19.5769527121826,7.62324053735219,0.));
#18310=CARTESIAN_POINT('Ctrl Pts',(19.6274933688524,7.6184403707059,0.));
#18311=CARTESIAN_POINT('Ctrl Pts',(19.6780827744426,7.61336212350879,0.));
#18312=CARTESIAN_POINT('Ctrl Pts',(19.7287195480601,7.60800746969261,0.));
#18313=CARTESIAN_POINT('Ctrl Pts',(19.7794022782484,7.60237814110186,0.));
#18314=CARTESIAN_POINT('Ctrl Pts',(19.830129556152,7.59647587605448,0.));
#18315=CARTESIAN_POINT('Ctrl Pts',(19.8808999994024,7.59030238888852,0.));
#18316=CARTESIAN_POINT('Ctrl Pts',(19.931712276832,7.58385933533351,0.));
#18317=CARTESIAN_POINT('Ctrl Pts',(19.9825651387294,7.57714827622806,0.));
#18318=CARTESIAN_POINT('Ctrl Pts',(20.0334574248556,7.57017066105973,0.));
#18319=CARTESIAN_POINT('Ctrl Pts',(20.0843880130978,7.5629278654946,0.));
#18320=CARTESIAN_POINT('Ctrl Pts',(20.1353557774357,7.55542122125494,0.));
#18321=CARTESIAN_POINT('Ctrl Pts',(20.1863595454674,7.54765204869254,0.));
#18322=CARTESIAN_POINT('Ctrl Pts',(20.2373980474879,7.53962169534167,0.));
#18323=CARTESIAN_POINT('Ctrl Pts',(20.2884698940944,7.53133155804008,0.));
#18324=CARTESIAN_POINT('Ctrl Pts',(20.3395736743243,7.52278303006887,0.));
#18325=CARTESIAN_POINT('Ctrl Pts',(20.3907080367098,7.51397746081993,0.));
#18326=CARTESIAN_POINT('Ctrl Pts',(20.4418717748497,7.50491611266253,0.));
#18327=CARTESIAN_POINT('Ctrl Pts',(20.4930639156161,7.49560012018405,0.));
#18328=CARTESIAN_POINT('Ctrl Pts',(20.5545277683621,7.48411651832412,0.));
#18329=CARTESIAN_POINT('Ctrl Pts',(20.6057817877246,7.47423073598682,0.));
#18330=CARTESIAN_POINT('Ctrl Pts',(20.6468066077586,7.46612041736313,0.));
#18331=CARTESIAN_POINT('Ctrl Pts',(20.6775873630604,7.45992433946823,0.));
#18332=CARTESIAN_POINT('Ctrl Pts',(20.698113262342,7.45574324794401,0.));
#18333=CARTESIAN_POINT('',(20.698113262342,7.45574324794407,13.));
#18334=CARTESIAN_POINT('Ctrl Pts',(20.698113262342,7.45574324794401,13.));
#18335=CARTESIAN_POINT('Ctrl Pts',(20.5970733923829,7.47632490126386,13.));
#18336=CARTESIAN_POINT('Ctrl Pts',(20.4961877829119,7.49544541992866,13.));
#18337=CARTESIAN_POINT('Ctrl Pts',(20.3954689812661,7.51308219876085,13.));
#18338=CARTESIAN_POINT('Ctrl Pts',(20.2285735541666,7.54230710699806,13.));
#18339=CARTESIAN_POINT('Ctrl Pts',(20.0621477284121,7.56745095724697,13.));
#18340=CARTESIAN_POINT('Ctrl Pts',(19.8963869092994,7.58830059943194,13.));
#18341=CARTESIAN_POINT('Ctrl Pts',(19.7689734227607,7.6043268571332,13.));
#18342=CARTESIAN_POINT('Ctrl Pts',(19.6419503907988,7.61781485456745,13.));
#18343=CARTESIAN_POINT('Ctrl Pts',(19.5154161608668,7.62864367960643,13.));
#18344=CARTESIAN_POINT('Ctrl Pts',(19.3792051088178,7.64030064904313,13.));
#18345=CARTESIAN_POINT('Ctrl Pts',(19.2435576419436,7.64888186449425,13.));
#18346=CARTESIAN_POINT('Ctrl Pts',(19.1086228815965,7.65417053749926,13.));
#18347=CARTESIAN_POINT('Ctrl Pts',(19.0339193340502,7.65709849049128,13.));
#18348=CARTESIAN_POINT('Ctrl Pts',(18.9594327293866,7.65902218177988,13.));
#18349=CARTESIAN_POINT('Ctrl Pts',(18.8851905383007,7.65990168002227,13.));
#18350=CARTESIAN_POINT('Ctrl Pts',(18.8136478507039,7.66074919902834,13.));
#18351=CARTESIAN_POINT('Ctrl Pts',(18.7423342826456,7.66062065570543,13.));
#18352=CARTESIAN_POINT('Ctrl Pts',(18.6712863103749,7.65944821272316,13.));
#18353=CARTESIAN_POINT('Ctrl Pts',(18.6098790735343,7.65843486242485,13.));
#18354=CARTESIAN_POINT('Ctrl Pts',(18.5486692004459,7.65664478986642,13.));
#18355=CARTESIAN_POINT('Ctrl Pts',(18.487665986183,7.65407864074932,13.));
#18356=CARTESIAN_POINT('Ctrl Pts',(18.4438867394649,7.65223703163625,13.));
#18357=CARTESIAN_POINT('Ctrl Pts',(18.4002130340387,7.64999840204417,13.));
#18358=CARTESIAN_POINT('Ctrl Pts',(18.3566609397295,7.64732656570801,13.));
#18359=CARTESIAN_POINT('Ctrl Pts',(18.3138180368763,7.64469823688926,13.));
#18360=CARTESIAN_POINT('Ctrl Pts',(18.2710948581547,7.64164464446501,13.));
#18361=CARTESIAN_POINT('Ctrl Pts',(18.2285117414039,7.63811742049252,13.));
#18362=CARTESIAN_POINT('Ctrl Pts',(18.1915896774841,7.63505911008904,13.));
#18363=CARTESIAN_POINT('Ctrl Pts',(18.1547737067871,7.63164238139629,13.));
#18364=CARTESIAN_POINT('Ctrl Pts',(18.1180614606597,7.62788266168324,13.));
#18365=CARTESIAN_POINT('Ctrl Pts',(18.0848085888946,7.62447721825009,13.));
#18366=CARTESIAN_POINT('Ctrl Pts',(18.0516390300359,7.62079564904865,13.));
#18367=CARTESIAN_POINT('Ctrl Pts',(18.0185473589474,7.61686093613286,13.));
#18368=CARTESIAN_POINT('Ctrl Pts',(17.9906726831367,7.61354654180559,13.));
#18369=CARTESIAN_POINT('Ctrl Pts',(17.9628527178424,7.61005417567813,13.));
#18370=CARTESIAN_POINT('Ctrl Pts',(17.935095231726,7.60636550506403,13.));
#18371=CARTESIAN_POINT('Ctrl Pts',(17.8949271289847,7.60102759731604,13.));
#18372=CARTESIAN_POINT('Ctrl Pts',(17.8548900766178,7.59527782595327,13.));
#18373=CARTESIAN_POINT('Ctrl Pts',(17.8150590775895,7.58891067819837,13.));
#18374=CARTESIAN_POINT('Ctrl Pts',(17.7909916428746,7.58506340053399,13.));
#18375=CARTESIAN_POINT('Ctrl Pts',(17.7670005714583,7.58098742033575,13.));
#18376=CARTESIAN_POINT('Ctrl Pts',(17.7430955910393,7.57665817615414,13.));
#18377=CARTESIAN_POINT('Ctrl Pts',(17.7210484741769,7.57266539512171,13.));
#18378=CARTESIAN_POINT('Ctrl Pts',(17.6990750115351,7.56845593261444,13.));
#18379=CARTESIAN_POINT('Ctrl Pts',(17.6771683090889,7.56405390347121,13.));
#18380=CARTESIAN_POINT('Ctrl Pts',(17.6470334199542,7.55799846630422,13.));
#18381=CARTESIAN_POINT('Ctrl Pts',(17.6170224065569,7.55158552706227,13.));
#18382=CARTESIAN_POINT('Ctrl Pts',(17.5870909090696,7.54495919888595,13.));
#18383=CARTESIAN_POINT('Ctrl Pts',(17.5681018330441,7.54075533806796,13.));
#18384=CARTESIAN_POINT('Ctrl Pts',(17.5491442492123,7.53646718588454,13.));
#18385=CARTESIAN_POINT('Ctrl Pts',(17.5302169634342,7.53210330805877,13.));
#18386=CARTESIAN_POINT('Ctrl Pts',(17.5132306054349,7.52818693083054,13.));
#18387=CARTESIAN_POINT('Ctrl Pts',(17.4962684162077,7.52421025223973,13.));
#18388=CARTESIAN_POINT('Ctrl Pts',(17.4793429836255,7.52014106533042,13.));
#18389=CARTESIAN_POINT('Ctrl Pts',(17.461550983085,7.51586353946286,13.));
#18390=CARTESIAN_POINT('Ctrl Pts',(17.4437995540587,7.51148394212765,13.));
#18391=CARTESIAN_POINT('Ctrl Pts',(17.4261238144457,7.50690601564176,13.));
#18392=CARTESIAN_POINT('Ctrl Pts',(17.3967644500333,7.4993020898714,13.));
#18393=CARTESIAN_POINT('Ctrl Pts',(17.3676168189686,7.49114308216385,13.));
#18394=CARTESIAN_POINT('Ctrl Pts',(17.3388922515559,7.48183975624005,13.));
#18395=CARTESIAN_POINT('Ctrl Pts',(17.3230525028126,7.47670957123173,13.));
#18396=CARTESIAN_POINT('Ctrl Pts',(17.3073418195136,7.47123011547027,13.));
#18397=CARTESIAN_POINT('Ctrl Pts',(17.2917860606183,7.46532888199725,13.));
#18398=CARTESIAN_POINT('Ctrl Pts',(17.2791322530438,7.46052853292248,13.));
#18399=CARTESIAN_POINT('Ctrl Pts',(17.266580931693,7.45544915949809,13.));
#18400=CARTESIAN_POINT('Ctrl Pts',(17.2541372868972,7.45007618140238,13.));
#18401=CARTESIAN_POINT('',(20.698113262342,7.45574324794407,0.));
#18402=CARTESIAN_POINT('Origin',(5.38923623413286E-12,1.75106900012182E-12,
0.));
#18403=CARTESIAN_POINT('',(21.1275013067528,6.1342227326009,0.));
#18404=CARTESIAN_POINT('Origin',(5.38923623413286E-12,1.75106900012182E-12,
0.));
#18405=CARTESIAN_POINT('',(21.1275013067528,6.1342227326009,13.));
#18406=CARTESIAN_POINT('Origin',(5.38923623413286E-12,1.75106900012182E-12,
13.));
#18407=CARTESIAN_POINT('',(21.1275013067528,6.1342227326009,0.));
#18408=CARTESIAN_POINT('Ctrl Pts',(18.337935196262,4.1144891981253,0.));
#18409=CARTESIAN_POINT('Ctrl Pts',(18.337935196262,4.1144891981253,21.));
#18410=CARTESIAN_POINT('Ctrl Pts',(18.3471320125699,4.11655269114951,0.));
#18411=CARTESIAN_POINT('Ctrl Pts',(18.3471320125699,4.11655269114951,21.));
#18412=CARTESIAN_POINT('Ctrl Pts',(18.3654573320481,4.1209201986886,0.));
#18413=CARTESIAN_POINT('Ctrl Pts',(18.3654573320481,4.1209201986886,21.));
#18414=CARTESIAN_POINT('Ctrl Pts',(18.3927403741815,4.12819301671078,0.));
#18415=CARTESIAN_POINT('Ctrl Pts',(18.3927403741815,4.12819301671078,21.));
#18416=CARTESIAN_POINT('Ctrl Pts',(18.4287286547442,4.13926275457062,0.));
#18417=CARTESIAN_POINT('Ctrl Pts',(18.4287286547442,4.13926275457062,21.));
#18418=CARTESIAN_POINT('Ctrl Pts',(18.4731856794913,4.15497867673974,0.));
#18419=CARTESIAN_POINT('Ctrl Pts',(18.4731856794913,4.15497867673974,21.));
#18420=CARTESIAN_POINT('Ctrl Pts',(18.5172668097744,4.17205262766561,0.));
#18421=CARTESIAN_POINT('Ctrl Pts',(18.5172668097744,4.17205262766561,21.));
#18422=CARTESIAN_POINT('Ctrl Pts',(18.5611217636409,4.1899696727862,0.));
#18423=CARTESIAN_POINT('Ctrl Pts',(18.5611217636409,4.1899696727862,21.));
#18424=CARTESIAN_POINT('Ctrl Pts',(18.6048602364653,4.20834600700665,0.));
#18425=CARTESIAN_POINT('Ctrl Pts',(18.6048602364653,4.20834600700665,21.));
#18426=CARTESIAN_POINT('Ctrl Pts',(18.6485210883348,4.22703266508919,0.));
#18427=CARTESIAN_POINT('Ctrl Pts',(18.6485210883348,4.22703266508919,21.));
#18428=CARTESIAN_POINT('Ctrl Pts',(18.6920958920047,4.24603817988452,0.));
#18429=CARTESIAN_POINT('Ctrl Pts',(18.6920958920047,4.24603817988452,21.));
#18430=CARTESIAN_POINT('Ctrl Pts',(18.735547949685,4.26546636161933,0.));
#18431=CARTESIAN_POINT('Ctrl Pts',(18.735547949685,4.26546636161933,21.));
#18432=CARTESIAN_POINT('Ctrl Pts',(18.778832216358,4.28545098663153,0.));
#18433=CARTESIAN_POINT('Ctrl Pts',(18.778832216358,4.28545098663153,21.));
#18434=CARTESIAN_POINT('Ctrl Pts',(18.8219166495975,4.30608591031526,0.));
#18435=CARTESIAN_POINT('Ctrl Pts',(18.8219166495975,4.30608591031526,21.));
#18436=CARTESIAN_POINT('Ctrl Pts',(18.8647973781745,4.32737526247704,0.));
#18437=CARTESIAN_POINT('Ctrl Pts',(18.8647973781745,4.32737526247704,21.));
#18438=CARTESIAN_POINT('Ctrl Pts',(18.9074876952706,4.34926881342021,0.));
#18439=CARTESIAN_POINT('Ctrl Pts',(18.9074876952706,4.34926881342021,21.));
#18440=CARTESIAN_POINT('Ctrl Pts',(18.9500107909187,4.37168516143122,0.));
#18441=CARTESIAN_POINT('Ctrl Pts',(18.9500107909187,4.37168516143122,21.));
#18442=CARTESIAN_POINT('Ctrl Pts',(18.9923914823906,4.39453820875555,0.));
#18443=CARTESIAN_POINT('Ctrl Pts',(18.9923914823906,4.39453820875555,21.));
#18444=CARTESIAN_POINT('Ctrl Pts',(19.034647328575,4.41776558033332,0.));
#18445=CARTESIAN_POINT('Ctrl Pts',(19.034647328575,4.41776558033332,21.));
#18446=CARTESIAN_POINT('Ctrl Pts',(19.0767833717249,4.44134542994081,0.));
#18447=CARTESIAN_POINT('Ctrl Pts',(19.0767833717249,4.44134542994081,21.));
#18448=CARTESIAN_POINT('Ctrl Pts',(19.1187970904932,4.46528051067021,0.));
#18449=CARTESIAN_POINT('Ctrl Pts',(19.1187970904932,4.46528051067021,21.));
#18450=CARTESIAN_POINT('Ctrl Pts',(19.1606814968494,4.48958819710577,0.));
#18451=CARTESIAN_POINT('Ctrl Pts',(19.1606814968494,4.48958819710577,21.));
#18452=CARTESIAN_POINT('Ctrl Pts',(19.2024287376926,4.51428889122954,0.));
#18453=CARTESIAN_POINT('Ctrl Pts',(19.2024287376926,4.51428889122954,21.));
#18454=CARTESIAN_POINT('Ctrl Pts',(19.2440340196551,4.53939338835151,0.));
#18455=CARTESIAN_POINT('Ctrl Pts',(19.2440340196551,4.53939338835151,21.));
#18456=CARTESIAN_POINT('Ctrl Pts',(19.2854975819105,4.56489651606741,0.));
#18457=CARTESIAN_POINT('Ctrl Pts',(19.2854975819105,4.56489651606741,21.));
#18458=CARTESIAN_POINT('Ctrl Pts',(19.3268225655679,4.59078395765677,0.));
#18459=CARTESIAN_POINT('Ctrl Pts',(19.3268225655679,4.59078395765677,21.));
#18460=CARTESIAN_POINT('Ctrl Pts',(19.3680137353983,4.61703633725712,0.));
#18461=CARTESIAN_POINT('Ctrl Pts',(19.3680137353983,4.61703633725712,21.));
#18462=CARTESIAN_POINT('Ctrl Pts',(19.4090759683639,4.64363405547472,0.));
#18463=CARTESIAN_POINT('Ctrl Pts',(19.4090759683639,4.64363405547472,21.));
#18464=CARTESIAN_POINT('Ctrl Pts',(19.4500125912299,4.67056260851453,0.));
#18465=CARTESIAN_POINT('Ctrl Pts',(19.4500125912299,4.67056260851453,21.));
#18466=CARTESIAN_POINT('Ctrl Pts',(19.4908246636763,4.69781487613784,0.));
#18467=CARTESIAN_POINT('Ctrl Pts',(19.4908246636763,4.69781487613784,21.));
#18468=CARTESIAN_POINT('Ctrl Pts',(19.531511899192,4.72538815796615,0.));
#18469=CARTESIAN_POINT('Ctrl Pts',(19.531511899192,4.72538815796615,21.));
#18470=CARTESIAN_POINT('Ctrl Pts',(19.5720732205813,4.75328238194611,0.));
#18471=CARTESIAN_POINT('Ctrl Pts',(19.5720732205813,4.75328238194611,21.));
#18472=CARTESIAN_POINT('Ctrl Pts',(19.6125074152527,4.7814979936173,0.));
#18473=CARTESIAN_POINT('Ctrl Pts',(19.6125074152527,4.7814979936173,21.));
#18474=CARTESIAN_POINT('Ctrl Pts',(19.6528138625329,4.81003361418061,0.));
#18475=CARTESIAN_POINT('Ctrl Pts',(19.6528138625329,4.81003361418061,21.));
#18476=CARTESIAN_POINT('Ctrl Pts',(19.6929928227072,4.83888510708974,0.));
#18477=CARTESIAN_POINT('Ctrl Pts',(19.6929928227072,4.83888510708974,21.));
#18478=CARTESIAN_POINT('Ctrl Pts',(19.7330450480715,4.86804682289087,0.));
#18479=CARTESIAN_POINT('Ctrl Pts',(19.7330450480715,4.86804682289087,21.));
#18480=CARTESIAN_POINT('Ctrl Pts',(19.772971552601,4.89751233527804,0.));
#18481=CARTESIAN_POINT('Ctrl Pts',(19.772971552601,4.89751233527804,21.));
#18482=CARTESIAN_POINT('Ctrl Pts',(19.8127733387903,4.92727531494346,0.));
#18483=CARTESIAN_POINT('Ctrl Pts',(19.8127733387903,4.92727531494346,21.));
#18484=CARTESIAN_POINT('Ctrl Pts',(19.8524510953961,4.95733049830096,0.));
#18485=CARTESIAN_POINT('Ctrl Pts',(19.8524510953961,4.95733049830096,21.));
#18486=CARTESIAN_POINT('Ctrl Pts',(19.8920050831202,4.98767405031333,0.));
#18487=CARTESIAN_POINT('Ctrl Pts',(19.8920050831202,4.98767405031333,21.));
#18488=CARTESIAN_POINT('Ctrl Pts',(19.931435301086,5.01830302225557,0.));
#18489=CARTESIAN_POINT('Ctrl Pts',(19.931435301086,5.01830302225557,21.));
#18490=CARTESIAN_POINT('Ctrl Pts',(19.9707415879783,5.04921502064063,0.));
#18491=CARTESIAN_POINT('Ctrl Pts',(19.9707415879783,5.04921502064063,21.));
#18492=CARTESIAN_POINT('Ctrl Pts',(20.0099237417205,5.08040781745336,0.));
#18493=CARTESIAN_POINT('Ctrl Pts',(20.0099237417205,5.08040781745336,21.));
#18494=CARTESIAN_POINT('Ctrl Pts',(20.0489816528155,5.11187891582334,0.));
#18495=CARTESIAN_POINT('Ctrl Pts',(20.0489816528155,5.11187891582334,21.));
#18496=CARTESIAN_POINT('Ctrl Pts',(20.087915358486,5.14362537555398,0.));
#18497=CARTESIAN_POINT('Ctrl Pts',(20.087915358486,5.14362537555398,21.));
#18498=CARTESIAN_POINT('Ctrl Pts',(20.1267249732337,5.17564404279922,0.));
#18499=CARTESIAN_POINT('Ctrl Pts',(20.1267249732337,5.17564404279922,21.));
#18500=CARTESIAN_POINT('Ctrl Pts',(20.1654106491899,5.20793168386163,0.));
#18501=CARTESIAN_POINT('Ctrl Pts',(20.1654106491899,5.20793168386163,21.));
#18502=CARTESIAN_POINT('Ctrl Pts',(20.2039725283917,5.2404851444189,0.));
#18503=CARTESIAN_POINT('Ctrl Pts',(20.2039725283917,5.2404851444189,21.));
#18504=CARTESIAN_POINT('Ctrl Pts',(20.2424106921768,5.2733015229815,0.));
#18505=CARTESIAN_POINT('Ctrl Pts',(20.2424106921768,5.2733015229815,21.));
#18506=CARTESIAN_POINT('Ctrl Pts',(20.2807251380077,5.30637824220997,0.));
#18507=CARTESIAN_POINT('Ctrl Pts',(20.2807251380077,5.30637824220997,21.));
#18508=CARTESIAN_POINT('Ctrl Pts',(20.3189158047642,5.33971294212214,0.));
#18509=CARTESIAN_POINT('Ctrl Pts',(20.3189158047642,5.33971294212214,21.));
#18510=CARTESIAN_POINT('Ctrl Pts',(20.3569825877537,5.37330341114649,0.));
#18511=CARTESIAN_POINT('Ctrl Pts',(20.3569825877537,5.37330341114649,21.));
#18512=CARTESIAN_POINT('Ctrl Pts',(20.3949253578015,5.40714750595875,0.));
#18513=CARTESIAN_POINT('Ctrl Pts',(20.3949253578015,5.40714750595875,21.));
#18514=CARTESIAN_POINT('Ctrl Pts',(20.4327439816542,5.44124306065111,0.));
#18515=CARTESIAN_POINT('Ctrl Pts',(20.4327439816542,5.44124306065111,21.));
#18516=CARTESIAN_POINT('Ctrl Pts',(20.4704383353718,5.47558784449851,0.));
#18517=CARTESIAN_POINT('Ctrl Pts',(20.4704383353718,5.47558784449851,21.));
#18518=CARTESIAN_POINT('Ctrl Pts',(20.5080083009242,5.51017962306782,0.));
#18519=CARTESIAN_POINT('Ctrl Pts',(20.5080083009242,5.51017962306782,21.));
#18520=CARTESIAN_POINT('Ctrl Pts',(20.5454537676144,5.5450161968946,0.));
#18521=CARTESIAN_POINT('Ctrl Pts',(20.5454537676144,5.5450161968946,21.));
#18522=CARTESIAN_POINT('Ctrl Pts',(20.5827746317185,5.58009544402475,0.));
#18523=CARTESIAN_POINT('Ctrl Pts',(20.5827746317185,5.58009544402475,21.));
#18524=CARTESIAN_POINT('Ctrl Pts',(20.6199707996366,5.61541536715149,0.));
#18525=CARTESIAN_POINT('Ctrl Pts',(20.6199707996366,5.61541536715149,21.));
#18526=CARTESIAN_POINT('Ctrl Pts',(20.6570421847033,5.65097411164335,0.));
#18527=CARTESIAN_POINT('Ctrl Pts',(20.6570421847033,5.65097411164335,21.));
#18528=CARTESIAN_POINT('Ctrl Pts',(20.6939886877061,5.68676990500163,0.));
#18529=CARTESIAN_POINT('Ctrl Pts',(20.6939886877061,5.68676990500163,21.));
#18530=CARTESIAN_POINT('Ctrl Pts',(20.7308101804425,5.72280100798241,0.));
#18531=CARTESIAN_POINT('Ctrl Pts',(20.7308101804425,5.72280100798241,21.));
#18532=CARTESIAN_POINT('Ctrl Pts',(20.7675064905026,5.75906566327796,0.));
#18533=CARTESIAN_POINT('Ctrl Pts',(20.7675064905026,5.75906566327796,21.));
#18534=CARTESIAN_POINT('Ctrl Pts',(20.8040773827343,5.79556203439644,0.));
#18535=CARTESIAN_POINT('Ctrl Pts',(20.8040773827343,5.79556203439644,21.));
#18536=CARTESIAN_POINT('Ctrl Pts',(20.8405225541277,5.83228817460178,0.));
#18537=CARTESIAN_POINT('Ctrl Pts',(20.8405225541277,5.83228817460178,21.));
#18538=CARTESIAN_POINT('Ctrl Pts',(20.8768416821402,5.86924212736287,0.));
#18539=CARTESIAN_POINT('Ctrl Pts',(20.8768416821402,5.86924212736287,21.));
#18540=CARTESIAN_POINT('Ctrl Pts',(20.9130344665641,5.90642200662599,0.));
#18541=CARTESIAN_POINT('Ctrl Pts',(20.9130344665641,5.90642200662599,21.));
#18542=CARTESIAN_POINT('Ctrl Pts',(20.9491006734021,5.94382608200804,0.));
#18543=CARTESIAN_POINT('Ctrl Pts',(20.9491006734021,5.94382608200804,21.));
#18544=CARTESIAN_POINT('Ctrl Pts',(20.9850401822713,5.98145286361836,0.));
#18545=CARTESIAN_POINT('Ctrl Pts',(20.9850401822713,5.98145286361836,21.));
#18546=CARTESIAN_POINT('Ctrl Pts',(21.0208530236003,6.01930117633044,0.));
#18547=CARTESIAN_POINT('Ctrl Pts',(21.0208530236003,6.01930117633044,21.));
#18548=CARTESIAN_POINT('Ctrl Pts',(21.0565393163693,6.05737013696532,0.));
#18549=CARTESIAN_POINT('Ctrl Pts',(21.0565393163693,6.05737013696532,21.));
#18550=CARTESIAN_POINT('Ctrl Pts',(21.0849872356853,6.08800133883114,0.));
#18551=CARTESIAN_POINT('Ctrl Pts',(21.0849872356853,6.08800133883114,21.));
#18552=CARTESIAN_POINT('Ctrl Pts',(21.1062663590356,6.11107360216958,0.));
#18553=CARTESIAN_POINT('Ctrl Pts',(21.1062663590356,6.11107360216958,21.));
#18554=CARTESIAN_POINT('Ctrl Pts',(21.1204271980506,6.12649903511517,0.));
#18555=CARTESIAN_POINT('Ctrl Pts',(21.1204271980506,6.12649903511517,21.));
#18556=CARTESIAN_POINT('Ctrl Pts',(21.1275013067528,6.1342227326009,0.));
#18557=CARTESIAN_POINT('Ctrl Pts',(21.1275013067528,6.1342227326009,21.));
#18558=CARTESIAN_POINT('Ctrl Pts',(18.337935196262,4.1144891981253,0.));
#18559=CARTESIAN_POINT('Ctrl Pts',(18.3471320125699,4.11655269114951,0.));
#18560=CARTESIAN_POINT('Ctrl Pts',(18.3654573320481,4.1209201986886,0.));
#18561=CARTESIAN_POINT('Ctrl Pts',(18.3927403741815,4.12819301671078,0.));
#18562=CARTESIAN_POINT('Ctrl Pts',(18.4287286547442,4.13926275457062,0.));
#18563=CARTESIAN_POINT('Ctrl Pts',(18.4731856794913,4.15497867673974,0.));
#18564=CARTESIAN_POINT('Ctrl Pts',(18.5172668097744,4.17205262766561,0.));
#18565=CARTESIAN_POINT('Ctrl Pts',(18.5611217636409,4.1899696727862,0.));
#18566=CARTESIAN_POINT('Ctrl Pts',(18.6048602364653,4.20834600700665,0.));
#18567=CARTESIAN_POINT('Ctrl Pts',(18.6485210883348,4.22703266508919,0.));
#18568=CARTESIAN_POINT('Ctrl Pts',(18.6920958920047,4.24603817988452,0.));
#18569=CARTESIAN_POINT('Ctrl Pts',(18.735547949685,4.26546636161933,0.));
#18570=CARTESIAN_POINT('Ctrl Pts',(18.778832216358,4.28545098663153,0.));
#18571=CARTESIAN_POINT('Ctrl Pts',(18.8219166495975,4.30608591031526,0.));
#18572=CARTESIAN_POINT('Ctrl Pts',(18.8647973781745,4.32737526247704,0.));
#18573=CARTESIAN_POINT('Ctrl Pts',(18.9074876952706,4.34926881342021,0.));
#18574=CARTESIAN_POINT('Ctrl Pts',(18.9500107909187,4.37168516143122,0.));
#18575=CARTESIAN_POINT('Ctrl Pts',(18.9923914823906,4.39453820875555,0.));
#18576=CARTESIAN_POINT('Ctrl Pts',(19.034647328575,4.41776558033332,0.));
#18577=CARTESIAN_POINT('Ctrl Pts',(19.0767833717249,4.44134542994081,0.));
#18578=CARTESIAN_POINT('Ctrl Pts',(19.1187970904932,4.46528051067021,0.));
#18579=CARTESIAN_POINT('Ctrl Pts',(19.1606814968494,4.48958819710577,0.));
#18580=CARTESIAN_POINT('Ctrl Pts',(19.2024287376926,4.51428889122954,0.));
#18581=CARTESIAN_POINT('Ctrl Pts',(19.2440340196551,4.53939338835151,0.));
#18582=CARTESIAN_POINT('Ctrl Pts',(19.2854975819105,4.56489651606741,0.));
#18583=CARTESIAN_POINT('Ctrl Pts',(19.3268225655679,4.59078395765677,0.));
#18584=CARTESIAN_POINT('Ctrl Pts',(19.3680137353983,4.61703633725712,0.));
#18585=CARTESIAN_POINT('Ctrl Pts',(19.4090759683639,4.64363405547472,0.));
#18586=CARTESIAN_POINT('Ctrl Pts',(19.4500125912299,4.67056260851453,0.));
#18587=CARTESIAN_POINT('Ctrl Pts',(19.4908246636763,4.69781487613784,0.));
#18588=CARTESIAN_POINT('Ctrl Pts',(19.531511899192,4.72538815796615,0.));
#18589=CARTESIAN_POINT('Ctrl Pts',(19.5720732205813,4.75328238194611,0.));
#18590=CARTESIAN_POINT('Ctrl Pts',(19.6125074152527,4.7814979936173,0.));
#18591=CARTESIAN_POINT('Ctrl Pts',(19.6528138625329,4.81003361418061,0.));
#18592=CARTESIAN_POINT('Ctrl Pts',(19.6929928227072,4.83888510708974,0.));
#18593=CARTESIAN_POINT('Ctrl Pts',(19.7330450480715,4.86804682289087,0.));
#18594=CARTESIAN_POINT('Ctrl Pts',(19.772971552601,4.89751233527804,0.));
#18595=CARTESIAN_POINT('Ctrl Pts',(19.8127733387903,4.92727531494346,0.));
#18596=CARTESIAN_POINT('Ctrl Pts',(19.8524510953961,4.95733049830096,0.));
#18597=CARTESIAN_POINT('Ctrl Pts',(19.8920050831202,4.98767405031333,0.));
#18598=CARTESIAN_POINT('Ctrl Pts',(19.931435301086,5.01830302225557,0.));
#18599=CARTESIAN_POINT('Ctrl Pts',(19.9707415879783,5.04921502064063,0.));
#18600=CARTESIAN_POINT('Ctrl Pts',(20.0099237417205,5.08040781745336,0.));
#18601=CARTESIAN_POINT('Ctrl Pts',(20.0489816528155,5.11187891582334,0.));
#18602=CARTESIAN_POINT('Ctrl Pts',(20.087915358486,5.14362537555398,0.));
#18603=CARTESIAN_POINT('Ctrl Pts',(20.1267249732337,5.17564404279922,0.));
#18604=CARTESIAN_POINT('Ctrl Pts',(20.1654106491899,5.20793168386163,0.));
#18605=CARTESIAN_POINT('Ctrl Pts',(20.2039725283917,5.2404851444189,0.));
#18606=CARTESIAN_POINT('Ctrl Pts',(20.2424106921768,5.2733015229815,0.));
#18607=CARTESIAN_POINT('Ctrl Pts',(20.2807251380077,5.30637824220997,0.));
#18608=CARTESIAN_POINT('Ctrl Pts',(20.3189158047642,5.33971294212214,0.));
#18609=CARTESIAN_POINT('Ctrl Pts',(20.3569825877537,5.37330341114649,0.));
#18610=CARTESIAN_POINT('Ctrl Pts',(20.3949253578015,5.40714750595875,0.));
#18611=CARTESIAN_POINT('Ctrl Pts',(20.4327439816542,5.44124306065111,0.));
#18612=CARTESIAN_POINT('Ctrl Pts',(20.4704383353718,5.47558784449851,0.));
#18613=CARTESIAN_POINT('Ctrl Pts',(20.5080083009242,5.51017962306782,0.));
#18614=CARTESIAN_POINT('Ctrl Pts',(20.5454537676144,5.5450161968946,0.));
#18615=CARTESIAN_POINT('Ctrl Pts',(20.5827746317185,5.58009544402475,0.));
#18616=CARTESIAN_POINT('Ctrl Pts',(20.6199707996366,5.61541536715149,0.));
#18617=CARTESIAN_POINT('Ctrl Pts',(20.6570421847033,5.65097411164335,0.));
#18618=CARTESIAN_POINT('Ctrl Pts',(20.6939886877061,5.68676990500163,0.));
#18619=CARTESIAN_POINT('Ctrl Pts',(20.7308101804425,5.72280100798241,0.));
#18620=CARTESIAN_POINT('Ctrl Pts',(20.7675064905026,5.75906566327796,0.));
#18621=CARTESIAN_POINT('Ctrl Pts',(20.8040773827343,5.79556203439644,0.));
#18622=CARTESIAN_POINT('Ctrl Pts',(20.8405225541277,5.83228817460178,0.));
#18623=CARTESIAN_POINT('Ctrl Pts',(20.8768416821402,5.86924212736287,0.));
#18624=CARTESIAN_POINT('Ctrl Pts',(20.9130344665641,5.90642200662599,0.));
#18625=CARTESIAN_POINT('Ctrl Pts',(20.9491006734021,5.94382608200804,0.));
#18626=CARTESIAN_POINT('Ctrl Pts',(20.9850401822713,5.98145286361836,0.));
#18627=CARTESIAN_POINT('Ctrl Pts',(21.0280155918661,6.02687083887286,0.));
#18628=CARTESIAN_POINT('Ctrl Pts',(21.0636702474951,6.06499496148844,0.));
#18629=CARTESIAN_POINT('Ctrl Pts',(21.0920928984154,6.09567013127871,0.));
#18630=CARTESIAN_POINT('Ctrl Pts',(21.1133530893457,6.11877533761502,0.));
#18631=CARTESIAN_POINT('Ctrl Pts',(21.1275013067528,6.1342227326009,0.));
#18632=CARTESIAN_POINT('Ctrl Pts',(18.337935196262,4.1144891981253,13.));
#18633=CARTESIAN_POINT('Ctrl Pts',(18.3534360435722,4.11796712888124,13.));
#18634=CARTESIAN_POINT('Ctrl Pts',(18.3688191549147,4.12185943359325,13.));
#18635=CARTESIAN_POINT('Ctrl Pts',(18.3840926405051,4.12613856044905,13.));
#18636=CARTESIAN_POINT('Ctrl Pts',(18.4019943079695,4.13115401717352,13.));
#18637=CARTESIAN_POINT('Ctrl Pts',(18.4197456248504,4.13670006308074,13.));
#18638=CARTESIAN_POINT('Ctrl Pts',(18.4373797424396,4.14266378080247,13.));
#18639=CARTESIAN_POINT('Ctrl Pts',(18.462191789787,4.15105501703698,13.));
#18640=CARTESIAN_POINT('Ctrl Pts',(18.4867739015687,4.16026629329012,13.));
#18641=CARTESIAN_POINT('Ctrl Pts',(18.5112408492841,4.16990400114915,13.));
#18642=CARTESIAN_POINT('Ctrl Pts',(18.5275152282521,4.17631459685994,13.));
#18643=CARTESIAN_POINT('Ctrl Pts',(18.5437392096415,4.18291190640452,13.));
#18644=CARTESIAN_POINT('Ctrl Pts',(18.5599376581282,4.18960898616729,13.));
#18645=CARTESIAN_POINT('Ctrl Pts',(18.5769891804621,4.19665876042442,13.));
#18646=CARTESIAN_POINT('Ctrl Pts',(18.59401265779,4.20381824254071,13.));
#18647=CARTESIAN_POINT('Ctrl Pts',(18.6110185062743,4.21104759333406,13.));
#18648=CARTESIAN_POINT('Ctrl Pts',(18.6299044319261,4.21907618312892,13.));
#18649=CARTESIAN_POINT('Ctrl Pts',(18.648768228348,4.22719219296854,13.));
#18650=CARTESIAN_POINT('Ctrl Pts',(18.6676042988209,4.23540730606195,13.));
#18651=CARTESIAN_POINT('Ctrl Pts',(18.6960005892894,4.24779198778028,13.));
#18652=CARTESIAN_POINT('Ctrl Pts',(18.7243319351414,4.26040793122445,13.));
#18653=CARTESIAN_POINT('Ctrl Pts',(18.7525479285473,4.27340283280954,13.));
#18654=CARTESIAN_POINT('Ctrl Pts',(18.7730462308896,4.28284334471236,13.));
#18655=CARTESIAN_POINT('Ctrl Pts',(18.793482731242,4.29248702329332,13.));
#18656=CARTESIAN_POINT('Ctrl Pts',(18.8138501272064,4.30235320730602,13.));
#18657=CARTESIAN_POINT('Ctrl Pts',(18.8387475247408,4.31441377243381,13.));
#18658=CARTESIAN_POINT('Ctrl Pts',(18.8635420328707,4.32680560861507,13.));
#18659=CARTESIAN_POINT('Ctrl Pts',(18.8882460103409,4.33948253067256,13.));
#18660=CARTESIAN_POINT('Ctrl Pts',(18.9149304060407,4.35317571043872,13.));
#18661=CARTESIAN_POINT('Ctrl Pts',(18.9415109548862,4.3671958076699,13.));
#18662=CARTESIAN_POINT('Ctrl Pts',(18.9680129070487,4.38145466526891,13.));
#18663=CARTESIAN_POINT('Ctrl Pts',(18.9924793847863,4.39461837562023,13.));
#18664=CARTESIAN_POINT('Ctrl Pts',(19.0168796293089,4.40798318216942,13.));
#18665=CARTESIAN_POINT('Ctrl Pts',(19.0412206987801,4.42152146521284,13.));
#18666=CARTESIAN_POINT('Ctrl Pts',(19.074289291449,4.43991391785044,13.));
#18667=CARTESIAN_POINT('Ctrl Pts',(19.1072480694626,4.45862842575511,13.));
#18668=CARTESIAN_POINT('Ctrl Pts',(19.1400849915655,4.47769255659232,13.));
#18669=CARTESIAN_POINT('Ctrl Pts',(19.1717719121569,4.49608903108798,13.));
#18670=CARTESIAN_POINT('Ctrl Pts',(19.2033430482091,4.51481852735374,13.));
#18671=CARTESIAN_POINT('Ctrl Pts',(19.2347910921211,4.53389559671967,13.));
#18672=CARTESIAN_POINT('Ctrl Pts',(19.2775141409376,4.55981232998548,13.));
#18673=CARTESIAN_POINT('Ctrl Pts',(19.3200109589111,4.5863674395711,13.));
#18674=CARTESIAN_POINT('Ctrl Pts',(19.3623013140095,4.61347737153013,13.));
#18675=CARTESIAN_POINT('Ctrl Pts',(19.3994736167756,4.63730641236946,13.));
#18676=CARTESIAN_POINT('Ctrl Pts',(19.4364884569407,4.66155758358413,13.));
#18677=CARTESIAN_POINT('Ctrl Pts',(19.4733518501762,4.68619912918312,13.));
#18678=CARTESIAN_POINT('Ctrl Pts',(19.5276974416099,4.7225267499439,13.));
#18679=CARTESIAN_POINT('Ctrl Pts',(19.5817111524207,4.75971143884683,13.));
#18680=CARTESIAN_POINT('Ctrl Pts',(19.635383906176,4.79774570279521,13.));
#18681=CARTESIAN_POINT('Ctrl Pts',(19.7031194451446,4.84574531502973,13.));
#18682=CARTESIAN_POINT('Ctrl Pts',(19.7703134645214,4.89509304253072,13.));
#18683=CARTESIAN_POINT('Ctrl Pts',(19.8369838016228,4.94566457604163,13.));
#18684=CARTESIAN_POINT('Ctrl Pts',(19.927293913377,5.01416761714691,13.));
#18685=CARTESIAN_POINT('Ctrl Pts',(20.0166413601247,5.08492180299973,13.));
#18686=CARTESIAN_POINT('Ctrl Pts',(20.1050225702956,5.15778644827742,13.));
#18687=CARTESIAN_POINT('Ctrl Pts',(20.1838167339246,5.22274718791513,13.));
#18688=CARTESIAN_POINT('Ctrl Pts',(20.2618454270691,5.28937724262181,13.));
#18689=CARTESIAN_POINT('Ctrl Pts',(20.3391090337862,5.35757729693952,13.));
#18690=CARTESIAN_POINT('Ctrl Pts',(20.4486128110626,5.45423552809844,13.));
#18691=CARTESIAN_POINT('Ctrl Pts',(20.55657724138,5.55405241094525,13.));
#18692=CARTESIAN_POINT('Ctrl Pts',(20.6629906951036,5.65680258457791,13.));
#18693=CARTESIAN_POINT('Ctrl Pts',(20.7456501415197,5.73661648192293,13.));
#18694=CARTESIAN_POINT('Ctrl Pts',(20.8273750326667,5.81820510886241,13.));
#18695=CARTESIAN_POINT('Ctrl Pts',(20.9081522149365,5.90147459235682,13.));
#18696=CARTESIAN_POINT('Ctrl Pts',(20.9780305832912,5.97350898965602,13.));
#18697=CARTESIAN_POINT('Ctrl Pts',(21.0471984365026,6.04679718413474,13.));
#18698=CARTESIAN_POINT('Ctrl Pts',(21.11565843993,6.12131239104349,13.));
#18699=CARTESIAN_POINT('Ctrl Pts',(21.1196084177252,6.12561173953841,13.));
#18700=CARTESIAN_POINT('Ctrl Pts',(21.1235560399575,6.12991518680116,13.));
#18701=CARTESIAN_POINT('Ctrl Pts',(21.1275013067528,6.1342227326009,13.));
#18702=CARTESIAN_POINT('Origin',(0.,0.,0.));
#18703=CARTESIAN_POINT('Origin',(0.,0.,0.));
#18704=CARTESIAN_POINT('Origin',(0.,0.,0.));
#18705=CARTESIAN_POINT('Origin',(0.,0.,0.));
#18706=CARTESIAN_POINT('Origin',(0.,0.,0.));
#18707=CARTESIAN_POINT('Origin',(0.,0.,0.));
#18708=CARTESIAN_POINT('Origin',(0.,0.,0.));
#18709=CARTESIAN_POINT('Origin',(0.,0.,0.));
#18710=CARTESIAN_POINT('Origin',(0.,0.,0.));
#18711=CARTESIAN_POINT('Origin',(0.,0.,0.));
#18712=CARTESIAN_POINT('Origin',(0.,0.,0.));
#18713=CARTESIAN_POINT('Origin',(0.,0.,0.));
#18714=CARTESIAN_POINT('Origin',(0.,0.,0.));
#18715=CARTESIAN_POINT('Origin',(0.,0.,0.));
#18716=CARTESIAN_POINT('Origin',(0.,0.,0.));
#18717=CARTESIAN_POINT('Origin',(0.,0.,0.));
#18718=CARTESIAN_POINT('Origin',(0.,0.,0.));
#18719=CARTESIAN_POINT('Origin',(0.,0.,0.));
#18720=CARTESIAN_POINT('',(17.4952923049513,2.59023998199238,0.));
#18721=CARTESIAN_POINT('Origin',(0.,0.,0.));
#18722=CARTESIAN_POINT('',(18.5778175999297,1.74105979901401,0.));
#18723=CARTESIAN_POINT('Origin',(18.4845093299966,2.73669706567396,0.));
#18724=CARTESIAN_POINT('',(18.7118598491961,1.75362185428836,0.));
#18725=CARTESIAN_POINT('',(17.5988843254813,1.64931697933718,0.));
#18726=CARTESIAN_POINT('',(21.9890268624765,0.694764450219646,0.));
#18727=CARTESIAN_POINT('Ctrl Pts',(18.7118598491961,1.75362185428836,0.));
#18728=CARTESIAN_POINT('Ctrl Pts',(18.7212441956871,1.75450132833464,0.));
#18729=CARTESIAN_POINT('Ctrl Pts',(18.7400222442427,1.75601041697575,0.));
#18730=CARTESIAN_POINT('Ctrl Pts',(18.7682173836138,1.75752447968136,0.));
#18731=CARTESIAN_POINT('Ctrl Pts',(18.8058650094752,1.7581175236483,0.));
#18732=CARTESIAN_POINT('Ctrl Pts',(18.8530026395886,1.75690876962597,0.));
#18733=CARTESIAN_POINT('Ctrl Pts',(18.9002024267872,1.75429229572775,0.));
#18734=CARTESIAN_POINT('Ctrl Pts',(18.947447637865,1.75080409924533,0.));
#18735=CARTESIAN_POINT('Ctrl Pts',(18.9947239970259,1.74684309825012,0.));
#18736=CARTESIAN_POINT('Ctrl Pts',(19.0420224296189,1.74256297552949,0.));
#18737=CARTESIAN_POINT('Ctrl Pts',(19.0893375576541,1.7379530116984,0.));
#18738=CARTESIAN_POINT('Ctrl Pts',(19.1366665585833,1.73290313712353,0.));
#18739=CARTESIAN_POINT('Ctrl Pts',(19.1840079312107,1.72727220327098,0.));
#18740=CARTESIAN_POINT('Ctrl Pts',(19.2313602042899,1.72096104670234,0.));
#18741=CARTESIAN_POINT('Ctrl Pts',(19.2787209722437,1.71396454346262,0.));
#18742=CARTESIAN_POINT('Ctrl Pts',(19.3260873558094,1.70633457265124,0.));
#18743=CARTESIAN_POINT('Ctrl Pts',(19.3734562555057,1.69815571801252,0.));
#18744=CARTESIAN_POINT('Ctrl Pts',(19.4208246682917,1.68951753233571,0.));
#18745=CARTESIAN_POINT('Ctrl Pts',(19.4681900187091,1.68048476382294,0.));
#18746=CARTESIAN_POINT('Ctrl Pts',(19.5155503513712,1.67107974760949,0.));
#18747=CARTESIAN_POINT('Ctrl Pts',(19.5629041190868,1.66129908621006,0.));
#18748=CARTESIAN_POINT('Ctrl Pts',(19.6102500448855,1.65112409599283,0.));
#18749=CARTESIAN_POINT('Ctrl Pts',(19.6575869645839,1.64053294677821,0.));
#18750=CARTESIAN_POINT('Ctrl Pts',(19.7049136553525,1.62951389038422,0.));
#18751=CARTESIAN_POINT('Ctrl Pts',(19.7522287462982,1.61807191996834,0.));
#18752=CARTESIAN_POINT('Ctrl Pts',(19.7995308006834,1.60622162219699,0.));
#18753=CARTESIAN_POINT('Ctrl Pts',(19.8468183626037,1.59398289700559,0.));
#18754=CARTESIAN_POINT('Ctrl Pts',(19.8940900137801,1.58137589158952,0.));
#18755=CARTESIAN_POINT('Ctrl Pts',(19.9413444362352,1.56841542790452,0.));
#18756=CARTESIAN_POINT('Ctrl Pts',(19.9885804375096,1.55510860515913,0.));
#18757=CARTESIAN_POINT('Ctrl Pts',(20.0357969106526,1.54145790302918,0.));
#18758=CARTESIAN_POINT('Ctrl Pts',(20.0829928089241,1.52746305716964,0.));
#18759=CARTESIAN_POINT('Ctrl Pts',(20.1301671167606,1.51312326913583,0.));
#18760=CARTESIAN_POINT('Ctrl Pts',(20.1773188177942,1.49843965844502,0.));
#18761=CARTESIAN_POINT('Ctrl Pts',(20.224446881308,1.48341623961914,0.));
#18762=CARTESIAN_POINT('Ctrl Pts',(20.2715502770004,1.46805861808021,0.));
#18763=CARTESIAN_POINT('Ctrl Pts',(20.3186279833818,1.45237321894404,0.));
#18764=CARTESIAN_POINT('Ctrl Pts',(20.3656789980171,1.43636637152782,0.));
#18765=CARTESIAN_POINT('Ctrl Pts',(20.4127023494155,1.4200432946371,0.));
#18766=CARTESIAN_POINT('Ctrl Pts',(20.4596971004275,1.40340771617024,0.));
#18767=CARTESIAN_POINT('Ctrl Pts',(20.5066623390132,1.38646244026049,0.));
#18768=CARTESIAN_POINT('Ctrl Pts',(20.5535971721246,1.36920969340018,0.));
#18769=CARTESIAN_POINT('Ctrl Pts',(20.6005007190809,1.35165153211253,0.));
#18770=CARTESIAN_POINT('Ctrl Pts',(20.6473721041685,1.3337902972259,0.));
#18771=CARTESIAN_POINT('Ctrl Pts',(20.694210454218,1.31562879653596,0.));
#18772=CARTESIAN_POINT('Ctrl Pts',(20.7410149035348,1.2971700649115,0.));
#18773=CARTESIAN_POINT('Ctrl Pts',(20.7877845975367,1.27841722479262,0.));
#18774=CARTESIAN_POINT('Ctrl Pts',(20.83451869657,1.25937332001005,0.));
#18775=CARTESIAN_POINT('Ctrl Pts',(20.881216381382,1.24004113517905,0.));
#18776=CARTESIAN_POINT('Ctrl Pts',(20.9278768531175,1.22042312071096,0.));
#18777=CARTESIAN_POINT('Ctrl Pts',(20.9744993243732,1.20052150219503,0.));
#18778=CARTESIAN_POINT('Ctrl Pts',(21.0210830121673,1.18033835060894,0.));
#18779=CARTESIAN_POINT('Ctrl Pts',(21.0676271313238,1.15987566445807,0.));
#18780=CARTESIAN_POINT('Ctrl Pts',(21.1141308858087,1.13913546246555,0.));
#18781=CARTESIAN_POINT('Ctrl Pts',(21.1605934684164,1.11811982787746,0.));
#18782=CARTESIAN_POINT('Ctrl Pts',(21.2070140764156,1.09683084929266,0.));
#18783=CARTESIAN_POINT('Ctrl Pts',(21.2533919248553,1.07527058431887,0.));
#18784=CARTESIAN_POINT('Ctrl Pts',(21.2997262593683,1.05344101900192,0.));
#18785=CARTESIAN_POINT('Ctrl Pts',(21.3460163737343,1.03134402396953,0.));
#18786=CARTESIAN_POINT('Ctrl Pts',(21.3922616124166,1.00898133629988,0.));
#18787=CARTESIAN_POINT('Ctrl Pts',(21.4384613333266,0.986354611081135,0.));
#18788=CARTESIAN_POINT('Ctrl Pts',(21.4846148770804,0.963465462815772,0.));
#18789=CARTESIAN_POINT('Ctrl Pts',(21.5307215366685,0.94031550952515,0.));
#18790=CARTESIAN_POINT('Ctrl Pts',(21.5767805209408,0.916906425150854,0.));
#18791=CARTESIAN_POINT('Ctrl Pts',(21.6227909401433,0.893239967513673,0.));
#18792=CARTESIAN_POINT('Ctrl Pts',(21.6687518829182,0.869317897714099,0.));
#18793=CARTESIAN_POINT('Ctrl Pts',(21.7146624809285,0.845141916726558,0.));
#18794=CARTESIAN_POINT('Ctrl Pts',(21.7605219769118,0.820713597934077,0.));
#18795=CARTESIAN_POINT('Ctrl Pts',(21.8063297959755,0.796034321106413,0.));
#18796=CARTESIAN_POINT('Ctrl Pts',(21.8612367655148,0.766119391688713,0.));
#18797=CARTESIAN_POINT('Ctrl Pts',(21.9069273598709,0.740879090965099,0.));
#18798=CARTESIAN_POINT('Ctrl Pts',(21.9434380560096,0.720488353007148,0.));
#18799=CARTESIAN_POINT('Ctrl Pts',(21.970797600548,0.705083756261759,0.));
#18800=CARTESIAN_POINT('Ctrl Pts',(21.9890268624765,0.694764450219581,0.));
#18801=CARTESIAN_POINT('',(21.9890268624765,-0.694764450219581,0.));
#18802=CARTESIAN_POINT('Origin',(5.6665783176868E-12,0.,0.));
#18803=CARTESIAN_POINT('',(18.7118598491961,-1.75362185428836,0.));
#18804=CARTESIAN_POINT('Ctrl Pts',(18.7118598491961,-1.75362185428836,0.));
#18805=CARTESIAN_POINT('Ctrl Pts',(18.7212441956871,-1.75450132833464,0.));
#18806=CARTESIAN_POINT('Ctrl Pts',(18.7400222442427,-1.75601041697575,0.));
#18807=CARTESIAN_POINT('Ctrl Pts',(18.7682173836138,-1.75752447968136,0.));
#18808=CARTESIAN_POINT('Ctrl Pts',(18.8058650094752,-1.7581175236483,0.));
#18809=CARTESIAN_POINT('Ctrl Pts',(18.8530026395886,-1.75690876962597,0.));
#18810=CARTESIAN_POINT('Ctrl Pts',(18.9002024267872,-1.75429229572775,0.));
#18811=CARTESIAN_POINT('Ctrl Pts',(18.947447637865,-1.75080409924533,0.));
#18812=CARTESIAN_POINT('Ctrl Pts',(18.9947239970259,-1.74684309825012,0.));
#18813=CARTESIAN_POINT('Ctrl Pts',(19.0420224296189,-1.74256297552949,0.));
#18814=CARTESIAN_POINT('Ctrl Pts',(19.0893375576541,-1.7379530116984,0.));
#18815=CARTESIAN_POINT('Ctrl Pts',(19.1366665585833,-1.73290313712353,0.));
#18816=CARTESIAN_POINT('Ctrl Pts',(19.1840079312107,-1.72727220327098,0.));
#18817=CARTESIAN_POINT('Ctrl Pts',(19.2313602042899,-1.72096104670234,0.));
#18818=CARTESIAN_POINT('Ctrl Pts',(19.2787209722437,-1.71396454346262,0.));
#18819=CARTESIAN_POINT('Ctrl Pts',(19.3260873558094,-1.70633457265124,0.));
#18820=CARTESIAN_POINT('Ctrl Pts',(19.3734562555057,-1.69815571801252,0.));
#18821=CARTESIAN_POINT('Ctrl Pts',(19.4208246682917,-1.68951753233571,0.));
#18822=CARTESIAN_POINT('Ctrl Pts',(19.4681900187091,-1.68048476382294,0.));
#18823=CARTESIAN_POINT('Ctrl Pts',(19.5155503513712,-1.67107974760949,0.));
#18824=CARTESIAN_POINT('Ctrl Pts',(19.5629041190868,-1.66129908621006,0.));
#18825=CARTESIAN_POINT('Ctrl Pts',(19.6102500448855,-1.65112409599283,0.));
#18826=CARTESIAN_POINT('Ctrl Pts',(19.6575869645839,-1.64053294677821,0.));
#18827=CARTESIAN_POINT('Ctrl Pts',(19.7049136553525,-1.62951389038422,0.));
#18828=CARTESIAN_POINT('Ctrl Pts',(19.7522287462982,-1.61807191996834,0.));
#18829=CARTESIAN_POINT('Ctrl Pts',(19.7995308006834,-1.60622162219699,0.));
#18830=CARTESIAN_POINT('Ctrl Pts',(19.8468183626037,-1.59398289700559,0.));
#18831=CARTESIAN_POINT('Ctrl Pts',(19.8940900137801,-1.58137589158952,0.));
#18832=CARTESIAN_POINT('Ctrl Pts',(19.9413444362352,-1.56841542790452,0.));
#18833=CARTESIAN_POINT('Ctrl Pts',(19.9885804375096,-1.55510860515913,0.));
#18834=CARTESIAN_POINT('Ctrl Pts',(20.0357969106526,-1.54145790302918,0.));
#18835=CARTESIAN_POINT('Ctrl Pts',(20.0829928089241,-1.52746305716964,0.));
#18836=CARTESIAN_POINT('Ctrl Pts',(20.1301671167606,-1.51312326913583,0.));
#18837=CARTESIAN_POINT('Ctrl Pts',(20.1773188177942,-1.49843965844502,0.));
#18838=CARTESIAN_POINT('Ctrl Pts',(20.224446881308,-1.48341623961914,0.));
#18839=CARTESIAN_POINT('Ctrl Pts',(20.2715502770004,-1.46805861808021,0.));
#18840=CARTESIAN_POINT('Ctrl Pts',(20.3186279833818,-1.45237321894404,0.));
#18841=CARTESIAN_POINT('Ctrl Pts',(20.3656789980171,-1.43636637152782,0.));
#18842=CARTESIAN_POINT('Ctrl Pts',(20.4127023494155,-1.4200432946371,0.));
#18843=CARTESIAN_POINT('Ctrl Pts',(20.4596971004275,-1.40340771617024,0.));
#18844=CARTESIAN_POINT('Ctrl Pts',(20.5066623390132,-1.38646244026049,0.));
#18845=CARTESIAN_POINT('Ctrl Pts',(20.5535971721246,-1.36920969340018,0.));
#18846=CARTESIAN_POINT('Ctrl Pts',(20.6005007190809,-1.35165153211253,0.));
#18847=CARTESIAN_POINT('Ctrl Pts',(20.6473721041685,-1.3337902972259,0.));
#18848=CARTESIAN_POINT('Ctrl Pts',(20.694210454218,-1.31562879653596,0.));
#18849=CARTESIAN_POINT('Ctrl Pts',(20.7410149035348,-1.2971700649115,0.));
#18850=CARTESIAN_POINT('Ctrl Pts',(20.7877845975367,-1.27841722479262,0.));
#18851=CARTESIAN_POINT('Ctrl Pts',(20.83451869657,-1.25937332001005,0.));
#18852=CARTESIAN_POINT('Ctrl Pts',(20.881216381382,-1.24004113517905,0.));
#18853=CARTESIAN_POINT('Ctrl Pts',(20.9278768531175,-1.22042312071096,0.));
#18854=CARTESIAN_POINT('Ctrl Pts',(20.9744993243732,-1.20052150219503,0.));
#18855=CARTESIAN_POINT('Ctrl Pts',(21.0210830121673,-1.18033835060894,0.));
#18856=CARTESIAN_POINT('Ctrl Pts',(21.0676271313238,-1.15987566445807,0.));
#18857=CARTESIAN_POINT('Ctrl Pts',(21.1141308858087,-1.13913546246555,0.));
#18858=CARTESIAN_POINT('Ctrl Pts',(21.1605934684164,-1.11811982787746,0.));
#18859=CARTESIAN_POINT('Ctrl Pts',(21.2070140764156,-1.09683084929266,0.));
#18860=CARTESIAN_POINT('Ctrl Pts',(21.2533919248553,-1.07527058431887,0.));
#18861=CARTESIAN_POINT('Ctrl Pts',(21.2997262593683,-1.05344101900192,0.));
#18862=CARTESIAN_POINT('Ctrl Pts',(21.3460163737343,-1.03134402396953,0.));
#18863=CARTESIAN_POINT('Ctrl Pts',(21.3922616124166,-1.00898133629988,0.));
#18864=CARTESIAN_POINT('Ctrl Pts',(21.4384613333266,-0.986354611081135,
0.));
#18865=CARTESIAN_POINT('Ctrl Pts',(21.4846148770804,-0.963465462815772,
0.));
#18866=CARTESIAN_POINT('Ctrl Pts',(21.5307215366685,-0.94031550952515,0.));
#18867=CARTESIAN_POINT('Ctrl Pts',(21.5767805209408,-0.916906425150854,
0.));
#18868=CARTESIAN_POINT('Ctrl Pts',(21.6227909401433,-0.893239967513673,
0.));
#18869=CARTESIAN_POINT('Ctrl Pts',(21.6687518829182,-0.869317897714099,
0.));
#18870=CARTESIAN_POINT('Ctrl Pts',(21.7146624809285,-0.845141916726558,
0.));
#18871=CARTESIAN_POINT('Ctrl Pts',(21.7605219769118,-0.820713597934077,
0.));
#18872=CARTESIAN_POINT('Ctrl Pts',(21.8063297959755,-0.796034321106413,
0.));
#18873=CARTESIAN_POINT('Ctrl Pts',(21.8612367655148,-0.766119391688713,
0.));
#18874=CARTESIAN_POINT('Ctrl Pts',(21.9069273598709,-0.740879090965099,
0.));
#18875=CARTESIAN_POINT('Ctrl Pts',(21.9434380560096,-0.720488353007148,
0.));
#18876=CARTESIAN_POINT('Ctrl Pts',(21.970797600548,-0.705083756261759,0.));
#18877=CARTESIAN_POINT('Ctrl Pts',(21.9890268624765,-0.694764450219581,
0.));
#18878=CARTESIAN_POINT('',(18.5778175999297,-1.74105979901401,0.));
#18879=CARTESIAN_POINT('',(17.5988843254813,-1.64931697933718,0.));
#18880=CARTESIAN_POINT('',(17.4952923049513,-2.59023998199238,0.));
#18881=CARTESIAN_POINT('Origin',(18.4845093299966,-2.73669706567396,0.));
#18882=CARTESIAN_POINT('Origin',(0.,0.,0.));
#18883=CARTESIAN_POINT('Origin',(0.,0.,0.));
#18884=CARTESIAN_POINT('Origin',(0.,0.,13.));
#18885=CARTESIAN_POINT('',(17.4952923049513,-2.59023998199238,13.));
#18886=CARTESIAN_POINT('Origin',(0.,0.,13.));
#18887=CARTESIAN_POINT('',(18.5778175999297,-1.74105979901401,13.));
#18888=CARTESIAN_POINT('Origin',(18.4845093299966,-2.73669706567396,13.));
#18889=CARTESIAN_POINT('',(18.7118598491961,-1.75362185428836,13.));
#18890=CARTESIAN_POINT('',(8.79944216274063,-0.824658489668591,13.));
#18891=CARTESIAN_POINT('',(21.9890268624765,-0.694764450219581,13.));
#18892=CARTESIAN_POINT('Ctrl Pts',(18.7118598491961,-1.75362185428836,13.));
#18893=CARTESIAN_POINT('Ctrl Pts',(18.7276767707323,-1.75510417082436,13.));
#18894=CARTESIAN_POINT('Ctrl Pts',(18.7435097673037,-1.75615601189521,13.));
#18895=CARTESIAN_POINT('Ctrl Pts',(18.7593580382054,-1.75680608702586,13.));
#18896=CARTESIAN_POINT('Ctrl Pts',(18.7779333970632,-1.75756802370092,13.));
#18897=CARTESIAN_POINT('Ctrl Pts',(18.7965297250933,-1.7577788791907,13.));
#18898=CARTESIAN_POINT('Ctrl Pts',(18.8151436576621,-1.75755628860662,13.));
#18899=CARTESIAN_POINT('Ctrl Pts',(18.8413343515946,-1.75724309300229,13.));
#18900=CARTESIAN_POINT('Ctrl Pts',(18.8675597701108,-1.75607893899569,13.));
#18901=CARTESIAN_POINT('Ctrl Pts',(18.8938074357046,-1.75447363677736,13.));
#18902=CARTESIAN_POINT('Ctrl Pts',(18.9112662728887,-1.75340585762722,13.));
#18903=CARTESIAN_POINT('Ctrl Pts',(18.9287348768749,-1.75214492936053,13.));
#18904=CARTESIAN_POINT('Ctrl Pts',(18.9462100283206,-1.75078122387692,13.));
#18905=CARTESIAN_POINT('Ctrl Pts',(18.9646054898042,-1.74934570031211,13.));
#18906=CARTESIAN_POINT('Ctrl Pts',(18.9830081804949,-1.74779717198946,13.));
#18907=CARTESIAN_POINT('Ctrl Pts',(19.0014156957677,-1.74617674699393,13.));
#18908=CARTESIAN_POINT('Ctrl Pts',(19.0218582491152,-1.74437717633347,13.));
#18909=CARTESIAN_POINT('Ctrl Pts',(19.0423067705939,-1.74248762596164,13.));
#18910=CARTESIAN_POINT('Ctrl Pts',(19.0627595477178,-1.74049525500507,13.));
#18911=CARTESIAN_POINT('Ctrl Pts',(19.093593101927,-1.73749165908643,13.));
#18912=CARTESIAN_POINT('Ctrl Pts',(19.1244363539391,-1.73424805120627,13.));
#18913=CARTESIAN_POINT('Ctrl Pts',(19.1552870037612,-1.73060838685053,13.));
#18914=CARTESIAN_POINT('Ctrl Pts',(19.1776993263911,-1.72796425026749,13.));
#18915=CARTESIAN_POINT('Ctrl Pts',(19.2001156537922,-1.72510779282615,13.));
#18916=CARTESIAN_POINT('Ctrl Pts',(19.2225350169744,-1.72201836571372,13.));
#18917=CARTESIAN_POINT('Ctrl Pts',(19.2499407687317,-1.71824180561129,13.));
#18918=CARTESIAN_POINT('Ctrl Pts',(19.2773510352358,-1.71411839344011,13.));
#18919=CARTESIAN_POINT('Ctrl Pts',(19.3047632983466,-1.70969587297614,13.));
#18920=CARTESIAN_POINT('Ctrl Pts',(19.3343730920125,-1.70491881688659,13.));
#18921=CARTESIAN_POINT('Ctrl Pts',(19.3639851445034,-1.69979875336899,13.));
#18922=CARTESIAN_POINT('Ctrl Pts',(19.393596228118,-1.69442732753702,13.));
#18923=CARTESIAN_POINT('Ctrl Pts',(19.420933041416,-1.68946845244065,13.));
#18924=CARTESIAN_POINT('Ctrl Pts',(19.4482690053259,-1.68429785630576,13.));
#18925=CARTESIAN_POINT('Ctrl Pts',(19.4756022976024,-1.67894398812401,13.));
#18926=CARTESIAN_POINT('Ctrl Pts',(19.5127359785892,-1.67167048330449,13.));
#18927=CARTESIAN_POINT('Ctrl Pts',(19.5498647401833,-1.66405675112972,13.));
#18928=CARTESIAN_POINT('Ctrl Pts',(19.5869856493472,-1.65607285223917,13.));
#18929=CARTESIAN_POINT('Ctrl Pts',(19.6228065249488,-1.64836856224694,13.));
#18930=CARTESIAN_POINT('Ctrl Pts',(19.6586201922964,-1.6403117703391,13.));
#18931=CARTESIAN_POINT('Ctrl Pts',(19.6944241980566,-1.63188637920554,13.));
#18932=CARTESIAN_POINT('Ctrl Pts',(19.743064943113,-1.62044024927043,13.));
#18933=CARTESIAN_POINT('Ctrl Pts',(19.7916877989836,-1.60831707819959,13.));
#18934=CARTESIAN_POINT('Ctrl Pts',(19.8402857465336,-1.59560243915671,13.));
#18935=CARTESIAN_POINT('Ctrl Pts',(19.8830022859205,-1.58442654785171,13.));
#18936=CARTESIAN_POINT('Ctrl Pts',(19.9256995149344,-1.57280052808225,13.));
#18937=CARTESIAN_POINT('Ctrl Pts',(19.9683733416779,-1.56075644053511,13.));
#18938=CARTESIAN_POINT('Ctrl Pts',(20.0312849226334,-1.54300053143161,13.));
#18939=CARTESIAN_POINT('Ctrl Pts',(20.0941457149814,-1.52432694533669,13.));
#18940=CARTESIAN_POINT('Ctrl Pts',(20.1569447710271,-1.50474000383683,13.));
#18941=CARTESIAN_POINT('Ctrl Pts',(20.23619779263,-1.48002109250969,13.));
#18942=CARTESIAN_POINT('Ctrl Pts',(20.3153523890243,-1.45385270861794,13.));
#18943=CARTESIAN_POINT('Ctrl Pts',(20.3943871108328,-1.4263585893238,13.));
#18944=CARTESIAN_POINT('Ctrl Pts',(20.50144573481,-1.38911568504398,13.));
#18945=CARTESIAN_POINT('Ctrl Pts',(20.6082844519443,-1.34943433504336,13.));
#18946=CARTESIAN_POINT('Ctrl Pts',(20.7148563913151,-1.30744723533842,13.));
#18947=CARTESIAN_POINT('Ctrl Pts',(20.8098680660179,-1.27001463645326,13.));
#18948=CARTESIAN_POINT('Ctrl Pts',(20.9046675817562,-1.23075788122755,13.));
#18949=CARTESIAN_POINT('Ctrl Pts',(20.9992246136264,-1.18977154295355,13.));
#18950=CARTESIAN_POINT('Ctrl Pts',(21.1332379306991,-1.13168263049381,13.));
#18951=CARTESIAN_POINT('Ctrl Pts',(21.2667633188666,-1.07011397738899,13.));
#18952=CARTESIAN_POINT('Ctrl Pts',(21.39972007734,-1.00527632083917,13.));
#18953=CARTESIAN_POINT('Ctrl Pts',(21.5029977296385,-0.954911969106397,
13.));
#18954=CARTESIAN_POINT('Ctrl Pts',(21.6059349886872,-0.902570955902035,
13.));
#18955=CARTESIAN_POINT('Ctrl Pts',(21.7084903363009,-0.848338495094938,
13.));
#18956=CARTESIAN_POINT('Ctrl Pts',(21.7972084616082,-0.801423318406783,
13.));
#18957=CARTESIAN_POINT('Ctrl Pts',(21.8856382915295,-0.75309614865077,13.));
#18958=CARTESIAN_POINT('Ctrl Pts',(21.9737740840291,-0.70338328327774,13.));
#18959=CARTESIAN_POINT('Ctrl Pts',(21.9788593171835,-0.700514964924581,
13.));
#18960=CARTESIAN_POINT('Ctrl Pts',(21.9839435766499,-0.697642020485719,
13.));
#18961=CARTESIAN_POINT('Ctrl Pts',(21.9890268624765,-0.694764450219581,
13.));
#18962=CARTESIAN_POINT('',(21.9890268624765,0.694764450219646,13.));
#18963=CARTESIAN_POINT('Origin',(5.6665783176868E-12,0.,13.));
#18964=CARTESIAN_POINT('',(18.7118598491961,1.75362185428836,13.));
#18965=CARTESIAN_POINT('Ctrl Pts',(21.9890268624765,0.694764450219581,13.));
#18966=CARTESIAN_POINT('Ctrl Pts',(21.899292315352,0.745561803242415,13.));
#18967=CARTESIAN_POINT('Ctrl Pts',(21.8092529632231,0.794921865484829,13.));
#18968=CARTESIAN_POINT('Ctrl Pts',(21.7189137539334,0.842819260803599,13.));
#18969=CARTESIAN_POINT('Ctrl Pts',(21.569217762881,0.922187323878742,13.));
#18970=CARTESIAN_POINT('Ctrl Pts',(21.4187072729658,0.997528955316443,13.));
#18971=CARTESIAN_POINT('Ctrl Pts',(21.2675022586751,1.06858105378595,13.));
#18972=CARTESIAN_POINT('Ctrl Pts',(21.151277217989,1.12319586318354,13.));
#18973=CARTESIAN_POINT('Ctrl Pts',(21.0346391561147,1.17527598651107,13.));
#18974=CARTESIAN_POINT('Ctrl Pts',(20.9176442431357,1.2246760384665,13.));
#18975=CARTESIAN_POINT('Ctrl Pts',(20.7917020384811,1.27785400402849,13.));
#18976=CARTESIAN_POINT('Ctrl Pts',(20.6653453749438,1.327932596435,13.));
#18977=CARTESIAN_POINT('Ctrl Pts',(20.5386490840353,1.37465955658916,13.));
#18978=CARTESIAN_POINT('Ctrl Pts',(20.4685065762054,1.40052887087594,13.));
#18979=CARTESIAN_POINT('Ctrl Pts',(20.3982600593864,1.42537603650614,13.));
#18980=CARTESIAN_POINT('Ctrl Pts',(20.3279233202978,1.4491545876062,13.));
#18981=CARTESIAN_POINT('Ctrl Pts',(20.2601440775423,1.47206853283981,13.));
#18982=CARTESIAN_POINT('Ctrl Pts',(20.1922811205662,1.49398338576682,13.));
#18983=CARTESIAN_POINT('Ctrl Pts',(20.1243481774567,1.51482335746684,13.));
#18984=CARTESIAN_POINT('Ctrl Pts',(20.0656332822855,1.53283548380392,13.));
#18985=CARTESIAN_POINT('Ctrl Pts',(20.0068660708186,1.55004791462172,13.));
#18986=CARTESIAN_POINT('Ctrl Pts',(19.948055582729,1.56645839168308,13.));
#18987=CARTESIAN_POINT('Ctrl Pts',(19.9058499563011,1.57823544857983,13.));
#18988=CARTESIAN_POINT('Ctrl Pts',(19.8636220195312,1.58960230250921,13.));
#18989=CARTESIAN_POINT('Ctrl Pts',(19.8213758735606,1.6005195724384,13.));
#18990=CARTESIAN_POINT('Ctrl Pts',(19.779817653503,1.61125906821305,13.));
#18991=CARTESIAN_POINT('Ctrl Pts',(19.7382418841798,1.62155711747599,13.));
#18992=CARTESIAN_POINT('Ctrl Pts',(19.6966529615092,1.63136143484286,13.));
#18993=CARTESIAN_POINT('Ctrl Pts',(19.6605929222238,1.63986235399904,13.));
#18994=CARTESIAN_POINT('Ctrl Pts',(19.6245230262468,1.64798961249865,13.));
#18995=CARTESIAN_POINT('Ctrl Pts',(19.5884457881434,1.65575861450053,13.));
#18996=CARTESIAN_POINT('Ctrl Pts',(19.5557680877664,1.66279554784111,13.));
#18997=CARTESIAN_POINT('Ctrl Pts',(19.5230842951169,1.66954412486476,13.));
#18998=CARTESIAN_POINT('Ctrl Pts',(19.4903963524289,1.67602787926304,13.));
#18999=CARTESIAN_POINT('Ctrl Pts',(19.4628617562097,1.68148945147165,13.));
#19000=CARTESIAN_POINT('Ctrl Pts',(19.4353241964729,1.68676485596096,13.));
#19001=CARTESIAN_POINT('Ctrl Pts',(19.4077853965428,1.69183425666145,13.));
#19002=CARTESIAN_POINT('Ctrl Pts',(19.3679337567804,1.6991702310336,13.));
#19003=CARTESIAN_POINT('Ctrl Pts',(19.3280794804744,1.70607400304418,13.));
#19004=CARTESIAN_POINT('Ctrl Pts',(19.2882303927414,1.71232694124141,13.));
#19005=CARTESIAN_POINT('Ctrl Pts',(19.2641520279257,1.71610520909267,13.));
#19006=CARTESIAN_POINT('Ctrl Pts',(19.2400756159532,1.71964237035168,13.));
#19007=CARTESIAN_POINT('Ctrl Pts',(19.2160028185096,1.72291205966735,13.));
#19008=CARTESIAN_POINT('Ctrl Pts',(19.1938009271707,1.72592763303679,13.));
#19009=CARTESIAN_POINT('Ctrl Pts',(19.1716021269002,1.72871436967202,13.));
#19010=CARTESIAN_POINT('Ctrl Pts',(19.1494073129856,1.7312973345182,13.));
#19011=CARTESIAN_POINT('Ctrl Pts',(19.1188760971263,1.73485046443309,13.));
#19012=CARTESIAN_POINT('Ctrl Pts',(19.0883522198778,1.73802530995667,13.));
#19013=CARTESIAN_POINT('Ctrl Pts',(19.0578380259466,1.74097263877354,13.));
#19014=CARTESIAN_POINT('Ctrl Pts',(19.0384792770224,1.74284247674769,13.));
#19015=CARTESIAN_POINT('Ctrl Pts',(19.0191244314898,1.74462241724651,13.));
#19016=CARTESIAN_POINT('Ctrl Pts',(18.9997750006083,1.74632097576622,13.));
#19017=CARTESIAN_POINT('Ctrl Pts',(18.9824097870281,1.74784535297679,13.));
#19018=CARTESIAN_POINT('Ctrl Pts',(18.9650489251703,1.74930491162225,13.));
#19019=CARTESIAN_POINT('Ctrl Pts',(18.9476944343168,1.75066513120051,13.));
#19020=CARTESIAN_POINT('Ctrl Pts',(18.9294514080686,1.75209499288178,13.));
#19021=CARTESIAN_POINT('Ctrl Pts',(18.9112154258052,1.75341524154102,13.));
#19022=CARTESIAN_POINT('Ctrl Pts',(18.8929901413736,1.75452347865357,13.));
#19023=CARTESIAN_POINT('Ctrl Pts',(18.8627179842696,1.75636425804473,13.));
#19024=CARTESIAN_POINT('Ctrl Pts',(18.8324756677938,1.75761169393965,13.));
#19025=CARTESIAN_POINT('Ctrl Pts',(18.8022820949853,1.75764008468142,13.));
#19026=CARTESIAN_POINT('Ctrl Pts',(18.78563228436,1.75765574034685,13.));
#19027=CARTESIAN_POINT('Ctrl Pts',(18.7689972916683,1.75729933637005,13.));
#19028=CARTESIAN_POINT('Ctrl Pts',(18.7523793043596,1.75649392367776,13.));
#19029=CARTESIAN_POINT('Ctrl Pts',(18.7388614288031,1.75583876199398,13.));
#19030=CARTESIAN_POINT('Ctrl Pts',(18.7253548001715,1.75488656240096,13.));
#19031=CARTESIAN_POINT('Ctrl Pts',(18.7118598491961,1.75362185428836,13.));
#19032=CARTESIAN_POINT('',(18.5778175999297,1.74105979901401,13.));
#19033=CARTESIAN_POINT('',(9.35592992459806,0.876810927144181,13.));
#19034=CARTESIAN_POINT('',(17.4952923049513,2.59023998199238,13.));
#19035=CARTESIAN_POINT('Origin',(18.4845093299966,2.73669706567396,13.));
#19036=CARTESIAN_POINT('Origin',(0.,0.,13.));
#19037=CARTESIAN_POINT('Origin',(0.,0.,13.));
#19038=CARTESIAN_POINT('Origin',(0.,0.,13.));
#19039=CARTESIAN_POINT('Origin',(0.,0.,13.));
#19040=CARTESIAN_POINT('Origin',(0.,0.,13.));
#19041=CARTESIAN_POINT('Origin',(0.,0.,13.));
#19042=CARTESIAN_POINT('Origin',(0.,0.,13.));
#19043=CARTESIAN_POINT('Origin',(0.,0.,13.));
#19044=CARTESIAN_POINT('Origin',(0.,0.,13.));
#19045=CARTESIAN_POINT('Origin',(0.,0.,13.));
#19046=CARTESIAN_POINT('Origin',(0.,0.,13.));
#19047=CARTESIAN_POINT('Origin',(0.,0.,13.));
#19048=CARTESIAN_POINT('Origin',(0.,0.,13.));
#19049=CARTESIAN_POINT('Origin',(0.,0.,13.));
#19050=CARTESIAN_POINT('Origin',(0.,0.,13.));
#19051=CARTESIAN_POINT('Origin',(0.,0.,13.));
#19052=CARTESIAN_POINT('Origin',(0.,0.,13.));
#19053=CARTESIAN_POINT('Origin',(0.,0.,13.));
#19054=CARTESIAN_POINT('Origin',(0.,0.,13.));
#19055=CARTESIAN_POINT('Origin',(0.,0.,0.));
#19056=CARTESIAN_POINT('',(17.4952923049513,2.59023998199238,0.));
#19057=CARTESIAN_POINT('Origin',(0.,0.,0.));
#19058=CARTESIAN_POINT('Origin',(0.,0.,0.));
#19059=CARTESIAN_POINT('Origin',(0.,0.,0.));
#19060=CARTESIAN_POINT('Origin',(0.,0.,0.));
#19061=CARTESIAN_POINT('Origin',(0.,0.,0.));
#19062=CARTESIAN_POINT('Origin',(0.,0.,0.));
#19063=CARTESIAN_POINT('Origin',(0.,0.,0.));
#19064=CARTESIAN_POINT('Origin',(0.,0.,0.));
#19065=CARTESIAN_POINT('Origin',(0.,0.,0.));
#19066=CARTESIAN_POINT('Origin',(0.,0.,0.));
#19067=CARTESIAN_POINT('Origin',(0.,0.,0.));
#19068=CARTESIAN_POINT('Origin',(0.,0.,0.));
#19069=CARTESIAN_POINT('Origin',(0.,0.,0.));
#19070=CARTESIAN_POINT('Origin',(0.,0.,0.));
#19071=CARTESIAN_POINT('Origin',(0.,0.,0.));
#19072=CARTESIAN_POINT('Origin',(0.,0.,0.));
#19073=CARTESIAN_POINT('Origin',(0.,0.,0.));
#19074=CARTESIAN_POINT('Origin',(0.,0.,0.));
#19075=CARTESIAN_POINT('Origin',(18.4845093299966,2.73669706567396,0.));
#19076=CARTESIAN_POINT('',(18.5778175999297,1.74105979901401,0.));
#19077=CARTESIAN_POINT('Origin',(18.7118598491961,1.75362185428836,0.));
#19078=CARTESIAN_POINT('',(18.7118598491961,1.75362185428836,0.));
#19079=CARTESIAN_POINT('Origin',(18.4845093299966,-2.73669706567396,0.));
#19080=CARTESIAN_POINT('',(18.5778175999297,-1.74105979901401,0.));
#19081=CARTESIAN_POINT('',(17.4952923049513,-2.59023998199238,0.));
#19082=CARTESIAN_POINT('Origin',(17.5988843254813,-1.64931697933718,0.));
#19083=CARTESIAN_POINT('',(18.7118598491961,-1.75362185428836,0.));
#19084=CARTESIAN_POINT('Ctrl Pts',(21.9890268624765,0.694764450219581,0.));
#19085=CARTESIAN_POINT('Ctrl Pts',(21.9890268624765,0.694764450219581,21.));
#19086=CARTESIAN_POINT('Ctrl Pts',(21.9799122315157,0.699924103234223,0.));
#19087=CARTESIAN_POINT('Ctrl Pts',(21.9799122315157,0.699924103234223,21.));
#19088=CARTESIAN_POINT('Ctrl Pts',(21.9616777523685,0.710218621843556,0.));
#19089=CARTESIAN_POINT('Ctrl Pts',(21.9616777523685,0.710218621843556,21.));
#19090=CARTESIAN_POINT('Ctrl Pts',(21.9343103819749,0.725586037496636,0.));
#19091=CARTESIAN_POINT('Ctrl Pts',(21.9343103819749,0.725586037496636,21.));
#19092=CARTESIAN_POINT('Ctrl Pts',(21.8977892409997,0.745927151109822,0.));
#19093=CARTESIAN_POINT('Ctrl Pts',(21.8977892409997,0.745927151109822,21.));
#19094=CARTESIAN_POINT('Ctrl Pts',(21.8520856039249,0.77110521325833,0.));
#19095=CARTESIAN_POINT('Ctrl Pts',(21.8520856039249,0.77110521325833,21.));
#19096=CARTESIAN_POINT('Ctrl Pts',(21.8063297959755,0.796034321106413,0.));
#19097=CARTESIAN_POINT('Ctrl Pts',(21.8063297959755,0.796034321106413,21.));
#19098=CARTESIAN_POINT('Ctrl Pts',(21.7605219769118,0.820713597934077,0.));
#19099=CARTESIAN_POINT('Ctrl Pts',(21.7605219769118,0.820713597934077,21.));
#19100=CARTESIAN_POINT('Ctrl Pts',(21.7146624809285,0.845141916726558,0.));
#19101=CARTESIAN_POINT('Ctrl Pts',(21.7146624809285,0.845141916726558,21.));
#19102=CARTESIAN_POINT('Ctrl Pts',(21.6687518829182,0.869317897714099,0.));
#19103=CARTESIAN_POINT('Ctrl Pts',(21.6687518829182,0.869317897714099,21.));
#19104=CARTESIAN_POINT('Ctrl Pts',(21.6227909401433,0.893239967513673,0.));
#19105=CARTESIAN_POINT('Ctrl Pts',(21.6227909401433,0.893239967513673,21.));
#19106=CARTESIAN_POINT('Ctrl Pts',(21.5767805209408,0.916906425150854,0.));
#19107=CARTESIAN_POINT('Ctrl Pts',(21.5767805209408,0.916906425150854,21.));
#19108=CARTESIAN_POINT('Ctrl Pts',(21.5307215366685,0.94031550952515,0.));
#19109=CARTESIAN_POINT('Ctrl Pts',(21.5307215366685,0.94031550952515,21.));
#19110=CARTESIAN_POINT('Ctrl Pts',(21.4846148770804,0.963465462815772,0.));
#19111=CARTESIAN_POINT('Ctrl Pts',(21.4846148770804,0.963465462815772,21.));
#19112=CARTESIAN_POINT('Ctrl Pts',(21.4384613333266,0.986354611081135,0.));
#19113=CARTESIAN_POINT('Ctrl Pts',(21.4384613333266,0.986354611081135,21.));
#19114=CARTESIAN_POINT('Ctrl Pts',(21.3922616124166,1.00898133629988,0.));
#19115=CARTESIAN_POINT('Ctrl Pts',(21.3922616124166,1.00898133629988,21.));
#19116=CARTESIAN_POINT('Ctrl Pts',(21.3460163737343,1.03134402396953,0.));
#19117=CARTESIAN_POINT('Ctrl Pts',(21.3460163737343,1.03134402396953,21.));
#19118=CARTESIAN_POINT('Ctrl Pts',(21.2997262593683,1.05344101900192,0.));
#19119=CARTESIAN_POINT('Ctrl Pts',(21.2997262593683,1.05344101900192,21.));
#19120=CARTESIAN_POINT('Ctrl Pts',(21.2533919248553,1.07527058431887,0.));
#19121=CARTESIAN_POINT('Ctrl Pts',(21.2533919248553,1.07527058431887,21.));
#19122=CARTESIAN_POINT('Ctrl Pts',(21.2070140764156,1.09683084929266,0.));
#19123=CARTESIAN_POINT('Ctrl Pts',(21.2070140764156,1.09683084929266,21.));
#19124=CARTESIAN_POINT('Ctrl Pts',(21.1605934684164,1.11811982787746,0.));
#19125=CARTESIAN_POINT('Ctrl Pts',(21.1605934684164,1.11811982787746,21.));
#19126=CARTESIAN_POINT('Ctrl Pts',(21.1141308858087,1.13913546246555,0.));
#19127=CARTESIAN_POINT('Ctrl Pts',(21.1141308858087,1.13913546246555,21.));
#19128=CARTESIAN_POINT('Ctrl Pts',(21.0676271313238,1.15987566445807,0.));
#19129=CARTESIAN_POINT('Ctrl Pts',(21.0676271313238,1.15987566445807,21.));
#19130=CARTESIAN_POINT('Ctrl Pts',(21.0210830121673,1.18033835060894,0.));
#19131=CARTESIAN_POINT('Ctrl Pts',(21.0210830121673,1.18033835060894,21.));
#19132=CARTESIAN_POINT('Ctrl Pts',(20.9744993243732,1.20052150219503,0.));
#19133=CARTESIAN_POINT('Ctrl Pts',(20.9744993243732,1.20052150219503,21.));
#19134=CARTESIAN_POINT('Ctrl Pts',(20.9278768531175,1.22042312071096,0.));
#19135=CARTESIAN_POINT('Ctrl Pts',(20.9278768531175,1.22042312071096,21.));
#19136=CARTESIAN_POINT('Ctrl Pts',(20.881216381382,1.24004113517905,0.));
#19137=CARTESIAN_POINT('Ctrl Pts',(20.881216381382,1.24004113517905,21.));
#19138=CARTESIAN_POINT('Ctrl Pts',(20.83451869657,1.25937332001005,0.));
#19139=CARTESIAN_POINT('Ctrl Pts',(20.83451869657,1.25937332001005,21.));
#19140=CARTESIAN_POINT('Ctrl Pts',(20.7877845975367,1.27841722479262,0.));
#19141=CARTESIAN_POINT('Ctrl Pts',(20.7877845975367,1.27841722479262,21.));
#19142=CARTESIAN_POINT('Ctrl Pts',(20.7410149035348,1.2971700649115,0.));
#19143=CARTESIAN_POINT('Ctrl Pts',(20.7410149035348,1.2971700649115,21.));
#19144=CARTESIAN_POINT('Ctrl Pts',(20.694210454218,1.31562879653596,0.));
#19145=CARTESIAN_POINT('Ctrl Pts',(20.694210454218,1.31562879653596,21.));
#19146=CARTESIAN_POINT('Ctrl Pts',(20.6473721041685,1.3337902972259,0.));
#19147=CARTESIAN_POINT('Ctrl Pts',(20.6473721041685,1.3337902972259,21.));
#19148=CARTESIAN_POINT('Ctrl Pts',(20.6005007190809,1.35165153211253,0.));
#19149=CARTESIAN_POINT('Ctrl Pts',(20.6005007190809,1.35165153211253,21.));
#19150=CARTESIAN_POINT('Ctrl Pts',(20.5535971721246,1.36920969340018,0.));
#19151=CARTESIAN_POINT('Ctrl Pts',(20.5535971721246,1.36920969340018,21.));
#19152=CARTESIAN_POINT('Ctrl Pts',(20.5066623390132,1.38646244026049,0.));
#19153=CARTESIAN_POINT('Ctrl Pts',(20.5066623390132,1.38646244026049,21.));
#19154=CARTESIAN_POINT('Ctrl Pts',(20.4596971004275,1.40340771617024,0.));
#19155=CARTESIAN_POINT('Ctrl Pts',(20.4596971004275,1.40340771617024,21.));
#19156=CARTESIAN_POINT('Ctrl Pts',(20.4127023494155,1.4200432946371,0.));
#19157=CARTESIAN_POINT('Ctrl Pts',(20.4127023494155,1.4200432946371,21.));
#19158=CARTESIAN_POINT('Ctrl Pts',(20.3656789980171,1.43636637152782,0.));
#19159=CARTESIAN_POINT('Ctrl Pts',(20.3656789980171,1.43636637152782,21.));
#19160=CARTESIAN_POINT('Ctrl Pts',(20.3186279833818,1.45237321894404,0.));
#19161=CARTESIAN_POINT('Ctrl Pts',(20.3186279833818,1.45237321894404,21.));
#19162=CARTESIAN_POINT('Ctrl Pts',(20.2715502770004,1.46805861808021,0.));
#19163=CARTESIAN_POINT('Ctrl Pts',(20.2715502770004,1.46805861808021,21.));
#19164=CARTESIAN_POINT('Ctrl Pts',(20.224446881308,1.48341623961914,0.));
#19165=CARTESIAN_POINT('Ctrl Pts',(20.224446881308,1.48341623961914,21.));
#19166=CARTESIAN_POINT('Ctrl Pts',(20.1773188177942,1.49843965844502,0.));
#19167=CARTESIAN_POINT('Ctrl Pts',(20.1773188177942,1.49843965844502,21.));
#19168=CARTESIAN_POINT('Ctrl Pts',(20.1301671167606,1.51312326913583,0.));
#19169=CARTESIAN_POINT('Ctrl Pts',(20.1301671167606,1.51312326913583,21.));
#19170=CARTESIAN_POINT('Ctrl Pts',(20.0829928089241,1.52746305716964,0.));
#19171=CARTESIAN_POINT('Ctrl Pts',(20.0829928089241,1.52746305716964,21.));
#19172=CARTESIAN_POINT('Ctrl Pts',(20.0357969106526,1.54145790302918,0.));
#19173=CARTESIAN_POINT('Ctrl Pts',(20.0357969106526,1.54145790302918,21.));
#19174=CARTESIAN_POINT('Ctrl Pts',(19.9885804375096,1.55510860515913,0.));
#19175=CARTESIAN_POINT('Ctrl Pts',(19.9885804375096,1.55510860515913,21.));
#19176=CARTESIAN_POINT('Ctrl Pts',(19.9413444362352,1.56841542790452,0.));
#19177=CARTESIAN_POINT('Ctrl Pts',(19.9413444362352,1.56841542790452,21.));
#19178=CARTESIAN_POINT('Ctrl Pts',(19.8940900137801,1.58137589158952,0.));
#19179=CARTESIAN_POINT('Ctrl Pts',(19.8940900137801,1.58137589158952,21.));
#19180=CARTESIAN_POINT('Ctrl Pts',(19.8468183626037,1.59398289700559,0.));
#19181=CARTESIAN_POINT('Ctrl Pts',(19.8468183626037,1.59398289700559,21.));
#19182=CARTESIAN_POINT('Ctrl Pts',(19.7995308006834,1.60622162219699,0.));
#19183=CARTESIAN_POINT('Ctrl Pts',(19.7995308006834,1.60622162219699,21.));
#19184=CARTESIAN_POINT('Ctrl Pts',(19.7522287462982,1.61807191996834,0.));
#19185=CARTESIAN_POINT('Ctrl Pts',(19.7522287462982,1.61807191996834,21.));
#19186=CARTESIAN_POINT('Ctrl Pts',(19.7049136553525,1.62951389038422,0.));
#19187=CARTESIAN_POINT('Ctrl Pts',(19.7049136553525,1.62951389038422,21.));
#19188=CARTESIAN_POINT('Ctrl Pts',(19.6575869645839,1.64053294677821,0.));
#19189=CARTESIAN_POINT('Ctrl Pts',(19.6575869645839,1.64053294677821,21.));
#19190=CARTESIAN_POINT('Ctrl Pts',(19.6102500448855,1.65112409599283,0.));
#19191=CARTESIAN_POINT('Ctrl Pts',(19.6102500448855,1.65112409599283,21.));
#19192=CARTESIAN_POINT('Ctrl Pts',(19.5629041190868,1.66129908621006,0.));
#19193=CARTESIAN_POINT('Ctrl Pts',(19.5629041190868,1.66129908621006,21.));
#19194=CARTESIAN_POINT('Ctrl Pts',(19.5155503513712,1.67107974760949,0.));
#19195=CARTESIAN_POINT('Ctrl Pts',(19.5155503513712,1.67107974760949,21.));
#19196=CARTESIAN_POINT('Ctrl Pts',(19.4681900187091,1.68048476382294,0.));
#19197=CARTESIAN_POINT('Ctrl Pts',(19.4681900187091,1.68048476382294,21.));
#19198=CARTESIAN_POINT('Ctrl Pts',(19.4208246682917,1.68951753233571,0.));
#19199=CARTESIAN_POINT('Ctrl Pts',(19.4208246682917,1.68951753233571,21.));
#19200=CARTESIAN_POINT('Ctrl Pts',(19.3734562555057,1.69815571801252,0.));
#19201=CARTESIAN_POINT('Ctrl Pts',(19.3734562555057,1.69815571801252,21.));
#19202=CARTESIAN_POINT('Ctrl Pts',(19.3260873558094,1.70633457265124,0.));
#19203=CARTESIAN_POINT('Ctrl Pts',(19.3260873558094,1.70633457265124,21.));
#19204=CARTESIAN_POINT('Ctrl Pts',(19.2787209722437,1.71396454346262,0.));
#19205=CARTESIAN_POINT('Ctrl Pts',(19.2787209722437,1.71396454346262,21.));
#19206=CARTESIAN_POINT('Ctrl Pts',(19.2313602042899,1.72096104670234,0.));
#19207=CARTESIAN_POINT('Ctrl Pts',(19.2313602042899,1.72096104670234,21.));
#19208=CARTESIAN_POINT('Ctrl Pts',(19.1840079312107,1.72727220327098,0.));
#19209=CARTESIAN_POINT('Ctrl Pts',(19.1840079312107,1.72727220327098,21.));
#19210=CARTESIAN_POINT('Ctrl Pts',(19.1366665585833,1.73290313712353,0.));
#19211=CARTESIAN_POINT('Ctrl Pts',(19.1366665585833,1.73290313712353,21.));
#19212=CARTESIAN_POINT('Ctrl Pts',(19.0893375576541,1.7379530116984,0.));
#19213=CARTESIAN_POINT('Ctrl Pts',(19.0893375576541,1.7379530116984,21.));
#19214=CARTESIAN_POINT('Ctrl Pts',(19.0420224296189,1.74256297552949,0.));
#19215=CARTESIAN_POINT('Ctrl Pts',(19.0420224296189,1.74256297552949,21.));
#19216=CARTESIAN_POINT('Ctrl Pts',(18.9947239970259,1.74684309825012,0.));
#19217=CARTESIAN_POINT('Ctrl Pts',(18.9947239970259,1.74684309825012,21.));
#19218=CARTESIAN_POINT('Ctrl Pts',(18.947447637865,1.75080409924533,0.));
#19219=CARTESIAN_POINT('Ctrl Pts',(18.947447637865,1.75080409924533,21.));
#19220=CARTESIAN_POINT('Ctrl Pts',(18.9002024267872,1.75429229572775,0.));
#19221=CARTESIAN_POINT('Ctrl Pts',(18.9002024267872,1.75429229572775,21.));
#19222=CARTESIAN_POINT('Ctrl Pts',(18.8530026395886,1.75690876962597,0.));
#19223=CARTESIAN_POINT('Ctrl Pts',(18.8530026395886,1.75690876962597,21.));
#19224=CARTESIAN_POINT('Ctrl Pts',(18.8058650094752,1.7581175236483,0.));
#19225=CARTESIAN_POINT('Ctrl Pts',(18.8058650094752,1.7581175236483,21.));
#19226=CARTESIAN_POINT('Ctrl Pts',(18.7682173836138,1.75752447968136,0.));
#19227=CARTESIAN_POINT('Ctrl Pts',(18.7682173836138,1.75752447968136,21.));
#19228=CARTESIAN_POINT('Ctrl Pts',(18.7400222442427,1.75601041697575,0.));
#19229=CARTESIAN_POINT('Ctrl Pts',(18.7400222442427,1.75601041697575,21.));
#19230=CARTESIAN_POINT('Ctrl Pts',(18.7212441956871,1.75450132833464,0.));
#19231=CARTESIAN_POINT('Ctrl Pts',(18.7212441956871,1.75450132833464,21.));
#19232=CARTESIAN_POINT('Ctrl Pts',(18.7118598491961,1.75362185428836,0.));
#19233=CARTESIAN_POINT('Ctrl Pts',(18.7118598491961,1.75362185428836,21.));
#19234=CARTESIAN_POINT('',(21.9890268624765,0.694764450219646,0.));
#19235=CARTESIAN_POINT('Origin',(5.6665783176868E-12,0.,0.));
#19236=CARTESIAN_POINT('',(21.9890268624765,-0.694764450219581,0.));
#19237=CARTESIAN_POINT('Ctrl Pts',(18.7118598491961,-1.75362185428836,0.));
#19238=CARTESIAN_POINT('Ctrl Pts',(18.7118598491961,-1.75362185428836,21.));
#19239=CARTESIAN_POINT('Ctrl Pts',(18.7212441956871,-1.75450132833464,0.));
#19240=CARTESIAN_POINT('Ctrl Pts',(18.7212441956871,-1.75450132833464,21.));
#19241=CARTESIAN_POINT('Ctrl Pts',(18.7400222442427,-1.75601041697575,0.));
#19242=CARTESIAN_POINT('Ctrl Pts',(18.7400222442427,-1.75601041697575,21.));
#19243=CARTESIAN_POINT('Ctrl Pts',(18.7682173836138,-1.75752447968136,0.));
#19244=CARTESIAN_POINT('Ctrl Pts',(18.7682173836138,-1.75752447968136,21.));
#19245=CARTESIAN_POINT('Ctrl Pts',(18.8058650094752,-1.7581175236483,0.));
#19246=CARTESIAN_POINT('Ctrl Pts',(18.8058650094752,-1.7581175236483,21.));
#19247=CARTESIAN_POINT('Ctrl Pts',(18.8530026395886,-1.75690876962597,0.));
#19248=CARTESIAN_POINT('Ctrl Pts',(18.8530026395886,-1.75690876962597,21.));
#19249=CARTESIAN_POINT('Ctrl Pts',(18.9002024267872,-1.75429229572775,0.));
#19250=CARTESIAN_POINT('Ctrl Pts',(18.9002024267872,-1.75429229572775,21.));
#19251=CARTESIAN_POINT('Ctrl Pts',(18.947447637865,-1.75080409924533,0.));
#19252=CARTESIAN_POINT('Ctrl Pts',(18.947447637865,-1.75080409924533,21.));
#19253=CARTESIAN_POINT('Ctrl Pts',(18.9947239970259,-1.74684309825012,0.));
#19254=CARTESIAN_POINT('Ctrl Pts',(18.9947239970259,-1.74684309825012,21.));
#19255=CARTESIAN_POINT('Ctrl Pts',(19.0420224296189,-1.74256297552949,0.));
#19256=CARTESIAN_POINT('Ctrl Pts',(19.0420224296189,-1.74256297552949,21.));
#19257=CARTESIAN_POINT('Ctrl Pts',(19.0893375576541,-1.7379530116984,0.));
#19258=CARTESIAN_POINT('Ctrl Pts',(19.0893375576541,-1.7379530116984,21.));
#19259=CARTESIAN_POINT('Ctrl Pts',(19.1366665585833,-1.73290313712353,0.));
#19260=CARTESIAN_POINT('Ctrl Pts',(19.1366665585833,-1.73290313712353,21.));
#19261=CARTESIAN_POINT('Ctrl Pts',(19.1840079312107,-1.72727220327098,0.));
#19262=CARTESIAN_POINT('Ctrl Pts',(19.1840079312107,-1.72727220327098,21.));
#19263=CARTESIAN_POINT('Ctrl Pts',(19.2313602042899,-1.72096104670234,0.));
#19264=CARTESIAN_POINT('Ctrl Pts',(19.2313602042899,-1.72096104670234,21.));
#19265=CARTESIAN_POINT('Ctrl Pts',(19.2787209722437,-1.71396454346262,0.));
#19266=CARTESIAN_POINT('Ctrl Pts',(19.2787209722437,-1.71396454346262,21.));
#19267=CARTESIAN_POINT('Ctrl Pts',(19.3260873558094,-1.70633457265124,0.));
#19268=CARTESIAN_POINT('Ctrl Pts',(19.3260873558094,-1.70633457265124,21.));
#19269=CARTESIAN_POINT('Ctrl Pts',(19.3734562555057,-1.69815571801252,0.));
#19270=CARTESIAN_POINT('Ctrl Pts',(19.3734562555057,-1.69815571801252,21.));
#19271=CARTESIAN_POINT('Ctrl Pts',(19.4208246682917,-1.68951753233571,0.));
#19272=CARTESIAN_POINT('Ctrl Pts',(19.4208246682917,-1.68951753233571,21.));
#19273=CARTESIAN_POINT('Ctrl Pts',(19.4681900187091,-1.68048476382294,0.));
#19274=CARTESIAN_POINT('Ctrl Pts',(19.4681900187091,-1.68048476382294,21.));
#19275=CARTESIAN_POINT('Ctrl Pts',(19.5155503513712,-1.67107974760949,0.));
#19276=CARTESIAN_POINT('Ctrl Pts',(19.5155503513712,-1.67107974760949,21.));
#19277=CARTESIAN_POINT('Ctrl Pts',(19.5629041190868,-1.66129908621006,0.));
#19278=CARTESIAN_POINT('Ctrl Pts',(19.5629041190868,-1.66129908621006,21.));
#19279=CARTESIAN_POINT('Ctrl Pts',(19.6102500448855,-1.65112409599283,0.));
#19280=CARTESIAN_POINT('Ctrl Pts',(19.6102500448855,-1.65112409599283,21.));
#19281=CARTESIAN_POINT('Ctrl Pts',(19.6575869645839,-1.64053294677821,0.));
#19282=CARTESIAN_POINT('Ctrl Pts',(19.6575869645839,-1.64053294677821,21.));
#19283=CARTESIAN_POINT('Ctrl Pts',(19.7049136553525,-1.62951389038422,0.));
#19284=CARTESIAN_POINT('Ctrl Pts',(19.7049136553525,-1.62951389038422,21.));
#19285=CARTESIAN_POINT('Ctrl Pts',(19.7522287462982,-1.61807191996834,0.));
#19286=CARTESIAN_POINT('Ctrl Pts',(19.7522287462982,-1.61807191996834,21.));
#19287=CARTESIAN_POINT('Ctrl Pts',(19.7995308006834,-1.60622162219699,0.));
#19288=CARTESIAN_POINT('Ctrl Pts',(19.7995308006834,-1.60622162219699,21.));
#19289=CARTESIAN_POINT('Ctrl Pts',(19.8468183626037,-1.59398289700559,0.));
#19290=CARTESIAN_POINT('Ctrl Pts',(19.8468183626037,-1.59398289700559,21.));
#19291=CARTESIAN_POINT('Ctrl Pts',(19.8940900137801,-1.58137589158952,0.));
#19292=CARTESIAN_POINT('Ctrl Pts',(19.8940900137801,-1.58137589158952,21.));
#19293=CARTESIAN_POINT('Ctrl Pts',(19.9413444362352,-1.56841542790452,0.));
#19294=CARTESIAN_POINT('Ctrl Pts',(19.9413444362352,-1.56841542790452,21.));
#19295=CARTESIAN_POINT('Ctrl Pts',(19.9885804375096,-1.55510860515913,0.));
#19296=CARTESIAN_POINT('Ctrl Pts',(19.9885804375096,-1.55510860515913,21.));
#19297=CARTESIAN_POINT('Ctrl Pts',(20.0357969106526,-1.54145790302918,0.));
#19298=CARTESIAN_POINT('Ctrl Pts',(20.0357969106526,-1.54145790302918,21.));
#19299=CARTESIAN_POINT('Ctrl Pts',(20.0829928089241,-1.52746305716964,0.));
#19300=CARTESIAN_POINT('Ctrl Pts',(20.0829928089241,-1.52746305716964,21.));
#19301=CARTESIAN_POINT('Ctrl Pts',(20.1301671167606,-1.51312326913583,0.));
#19302=CARTESIAN_POINT('Ctrl Pts',(20.1301671167606,-1.51312326913583,21.));
#19303=CARTESIAN_POINT('Ctrl Pts',(20.1773188177942,-1.49843965844502,0.));
#19304=CARTESIAN_POINT('Ctrl Pts',(20.1773188177942,-1.49843965844502,21.));
#19305=CARTESIAN_POINT('Ctrl Pts',(20.224446881308,-1.48341623961914,0.));
#19306=CARTESIAN_POINT('Ctrl Pts',(20.224446881308,-1.48341623961914,21.));
#19307=CARTESIAN_POINT('Ctrl Pts',(20.2715502770004,-1.46805861808021,0.));
#19308=CARTESIAN_POINT('Ctrl Pts',(20.2715502770004,-1.46805861808021,21.));
#19309=CARTESIAN_POINT('Ctrl Pts',(20.3186279833818,-1.45237321894404,0.));
#19310=CARTESIAN_POINT('Ctrl Pts',(20.3186279833818,-1.45237321894404,21.));
#19311=CARTESIAN_POINT('Ctrl Pts',(20.3656789980171,-1.43636637152782,0.));
#19312=CARTESIAN_POINT('Ctrl Pts',(20.3656789980171,-1.43636637152782,21.));
#19313=CARTESIAN_POINT('Ctrl Pts',(20.4127023494155,-1.4200432946371,0.));
#19314=CARTESIAN_POINT('Ctrl Pts',(20.4127023494155,-1.4200432946371,21.));
#19315=CARTESIAN_POINT('Ctrl Pts',(20.4596971004275,-1.40340771617024,0.));
#19316=CARTESIAN_POINT('Ctrl Pts',(20.4596971004275,-1.40340771617024,21.));
#19317=CARTESIAN_POINT('Ctrl Pts',(20.5066623390132,-1.38646244026049,0.));
#19318=CARTESIAN_POINT('Ctrl Pts',(20.5066623390132,-1.38646244026049,21.));
#19319=CARTESIAN_POINT('Ctrl Pts',(20.5535971721246,-1.36920969340018,0.));
#19320=CARTESIAN_POINT('Ctrl Pts',(20.5535971721246,-1.36920969340018,21.));
#19321=CARTESIAN_POINT('Ctrl Pts',(20.6005007190809,-1.35165153211253,0.));
#19322=CARTESIAN_POINT('Ctrl Pts',(20.6005007190809,-1.35165153211253,21.));
#19323=CARTESIAN_POINT('Ctrl Pts',(20.6473721041685,-1.3337902972259,0.));
#19324=CARTESIAN_POINT('Ctrl Pts',(20.6473721041685,-1.3337902972259,21.));
#19325=CARTESIAN_POINT('Ctrl Pts',(20.694210454218,-1.31562879653596,0.));
#19326=CARTESIAN_POINT('Ctrl Pts',(20.694210454218,-1.31562879653596,21.));
#19327=CARTESIAN_POINT('Ctrl Pts',(20.7410149035348,-1.2971700649115,0.));
#19328=CARTESIAN_POINT('Ctrl Pts',(20.7410149035348,-1.2971700649115,21.));
#19329=CARTESIAN_POINT('Ctrl Pts',(20.7877845975367,-1.27841722479262,0.));
#19330=CARTESIAN_POINT('Ctrl Pts',(20.7877845975367,-1.27841722479262,21.));
#19331=CARTESIAN_POINT('Ctrl Pts',(20.83451869657,-1.25937332001005,0.));
#19332=CARTESIAN_POINT('Ctrl Pts',(20.83451869657,-1.25937332001005,21.));
#19333=CARTESIAN_POINT('Ctrl Pts',(20.881216381382,-1.24004113517905,0.));
#19334=CARTESIAN_POINT('Ctrl Pts',(20.881216381382,-1.24004113517905,21.));
#19335=CARTESIAN_POINT('Ctrl Pts',(20.9278768531175,-1.22042312071096,0.));
#19336=CARTESIAN_POINT('Ctrl Pts',(20.9278768531175,-1.22042312071096,21.));
#19337=CARTESIAN_POINT('Ctrl Pts',(20.9744993243732,-1.20052150219503,0.));
#19338=CARTESIAN_POINT('Ctrl Pts',(20.9744993243732,-1.20052150219503,21.));
#19339=CARTESIAN_POINT('Ctrl Pts',(21.0210830121673,-1.18033835060894,0.));
#19340=CARTESIAN_POINT('Ctrl Pts',(21.0210830121673,-1.18033835060894,21.));
#19341=CARTESIAN_POINT('Ctrl Pts',(21.0676271313238,-1.15987566445807,0.));
#19342=CARTESIAN_POINT('Ctrl Pts',(21.0676271313238,-1.15987566445807,21.));
#19343=CARTESIAN_POINT('Ctrl Pts',(21.1141308858087,-1.13913546246555,0.));
#19344=CARTESIAN_POINT('Ctrl Pts',(21.1141308858087,-1.13913546246555,21.));
#19345=CARTESIAN_POINT('Ctrl Pts',(21.1605934684164,-1.11811982787746,0.));
#19346=CARTESIAN_POINT('Ctrl Pts',(21.1605934684164,-1.11811982787746,21.));
#19347=CARTESIAN_POINT('Ctrl Pts',(21.2070140764156,-1.09683084929266,0.));
#19348=CARTESIAN_POINT('Ctrl Pts',(21.2070140764156,-1.09683084929266,21.));
#19349=CARTESIAN_POINT('Ctrl Pts',(21.2533919248553,-1.07527058431887,0.));
#19350=CARTESIAN_POINT('Ctrl Pts',(21.2533919248553,-1.07527058431887,21.));
#19351=CARTESIAN_POINT('Ctrl Pts',(21.2997262593683,-1.05344101900192,0.));
#19352=CARTESIAN_POINT('Ctrl Pts',(21.2997262593683,-1.05344101900192,21.));
#19353=CARTESIAN_POINT('Ctrl Pts',(21.3460163737343,-1.03134402396953,0.));
#19354=CARTESIAN_POINT('Ctrl Pts',(21.3460163737343,-1.03134402396953,21.));
#19355=CARTESIAN_POINT('Ctrl Pts',(21.3922616124166,-1.00898133629988,0.));
#19356=CARTESIAN_POINT('Ctrl Pts',(21.3922616124166,-1.00898133629988,21.));
#19357=CARTESIAN_POINT('Ctrl Pts',(21.4384613333266,-0.986354611081135,
0.));
#19358=CARTESIAN_POINT('Ctrl Pts',(21.4384613333266,-0.986354611081135,
21.));
#19359=CARTESIAN_POINT('Ctrl Pts',(21.4846148770804,-0.963465462815772,
0.));
#19360=CARTESIAN_POINT('Ctrl Pts',(21.4846148770804,-0.963465462815772,
21.));
#19361=CARTESIAN_POINT('Ctrl Pts',(21.5307215366685,-0.94031550952515,0.));
#19362=CARTESIAN_POINT('Ctrl Pts',(21.5307215366685,-0.94031550952515,21.));
#19363=CARTESIAN_POINT('Ctrl Pts',(21.5767805209408,-0.916906425150854,
0.));
#19364=CARTESIAN_POINT('Ctrl Pts',(21.5767805209408,-0.916906425150854,
21.));
#19365=CARTESIAN_POINT('Ctrl Pts',(21.6227909401433,-0.893239967513673,
0.));
#19366=CARTESIAN_POINT('Ctrl Pts',(21.6227909401433,-0.893239967513673,
21.));
#19367=CARTESIAN_POINT('Ctrl Pts',(21.6687518829182,-0.869317897714099,
0.));
#19368=CARTESIAN_POINT('Ctrl Pts',(21.6687518829182,-0.869317897714099,
21.));
#19369=CARTESIAN_POINT('Ctrl Pts',(21.7146624809285,-0.845141916726558,
0.));
#19370=CARTESIAN_POINT('Ctrl Pts',(21.7146624809285,-0.845141916726558,
21.));
#19371=CARTESIAN_POINT('Ctrl Pts',(21.7605219769118,-0.820713597934077,
0.));
#19372=CARTESIAN_POINT('Ctrl Pts',(21.7605219769118,-0.820713597934077,
21.));
#19373=CARTESIAN_POINT('Ctrl Pts',(21.8063297959755,-0.796034321106413,
0.));
#19374=CARTESIAN_POINT('Ctrl Pts',(21.8063297959755,-0.796034321106413,
21.));
#19375=CARTESIAN_POINT('Ctrl Pts',(21.8520856039249,-0.77110521325833,0.));
#19376=CARTESIAN_POINT('Ctrl Pts',(21.8520856039249,-0.77110521325833,21.));
#19377=CARTESIAN_POINT('Ctrl Pts',(21.8977892409997,-0.745927151109822,
0.));
#19378=CARTESIAN_POINT('Ctrl Pts',(21.8977892409997,-0.745927151109822,
21.));
#19379=CARTESIAN_POINT('Ctrl Pts',(21.9343103819749,-0.725586037496636,
0.));
#19380=CARTESIAN_POINT('Ctrl Pts',(21.9343103819749,-0.725586037496636,
21.));
#19381=CARTESIAN_POINT('Ctrl Pts',(21.9616777523685,-0.710218621843556,
0.));
#19382=CARTESIAN_POINT('Ctrl Pts',(21.9616777523685,-0.710218621843556,
21.));
#19383=CARTESIAN_POINT('Ctrl Pts',(21.9799122315157,-0.699924103234223,
0.));
#19384=CARTESIAN_POINT('Ctrl Pts',(21.9799122315157,-0.699924103234223,
21.));
#19385=CARTESIAN_POINT('Ctrl Pts',(21.9890268624765,-0.694764450219581,
0.));
#19386=CARTESIAN_POINT('Ctrl Pts',(21.9890268624765,-0.694764450219581,
21.));
#19387=CARTESIAN_POINT('Origin',(0.,0.,0.));
#19388=CARTESIAN_POINT('',(0.,0.,0.));
#19389=CARTESIAN_POINT('Origin',(-8.50613908013701E-14,0.,-14.2400000000013));
#19390=CARTESIAN_POINT('',(7.91099999999991,9.68818082805471E-16,-13.6663636363649));
#19391=CARTESIAN_POINT('Origin',(-8.5106502022526E-14,0.,-13.6663636363649));
#19392=CARTESIAN_POINT('',(6.39999999999992,-7.83773951454306E-16,-15.0400000000013));
#19393=CARTESIAN_POINT('',(7.27999999999992,8.91542869779273E-16,-14.2400000000013));
#19394=CARTESIAN_POINT('Origin',(-8.4998478163308E-14,0.,-15.0400000000013));
#19395=CARTESIAN_POINT('Origin',(-8.67707890235993E-14,0.,7.49678643762621));
#19396=CARTESIAN_POINT('',(7.91099999999991,9.68818082805471E-16,7.49678643762622));
#19397=CARTESIAN_POINT('Origin',(-8.67707890235993E-14,0.,7.49678643762621));
#19398=CARTESIAN_POINT('',(8.2038932188134,-2.00937431419332E-15,8.20389321881279));
#19399=CARTESIAN_POINT('Origin',(8.91099999999991,-1.09128276272021E-15,
7.49678643762621));
#19400=CARTESIAN_POINT('Origin',(-8.54871728961371E-14,-5.02343578548331E-16,
8.20389321881279));
#19401=CARTESIAN_POINT('Origin',(-8.70651583236477E-14,0.,11.239999999999));
#19402=CARTESIAN_POINT('',(14.4799999999999,-1.77328856516537E-15,14.4799999999987));
#19403=CARTESIAN_POINT('Origin',(-8.73199545077991E-14,0.,14.4799999999987));
#19404=CARTESIAN_POINT('',(11.2399999999999,1.37650300224163E-15,11.239999999999));
#19405=CARTESIAN_POINT('Origin',(-8.59044201514021E-14,0.,-3.52000000000102));
#19406=CARTESIAN_POINT('',(7.91099999999991,-9.68818082805471E-16,-3.52000000000102));
#19407=CARTESIAN_POINT('Origin',(5.,2.88675134594813,10.1599999999987));
#19408=CARTESIAN_POINT('',(5.,2.88675134594813,10.1599999999987));
#19409=CARTESIAN_POINT('',(2.77555756156289E-15,3.60822483003176E-15,7.2732486540506));
#19410=CARTESIAN_POINT('',(3.99999999999999,2.3094010767585,9.5826497308091));
#19411=CARTESIAN_POINT('',(-5.55111512312578E-16,5.77350269189626,10.1599999999987));
#19412=CARTESIAN_POINT('',(-2.13056424354826E-15,5.77350269189626,10.1599999999987));
#19413=CARTESIAN_POINT('',(-1.66533453693773E-15,4.61880215351701,9.5826497308091));
#19414=CARTESIAN_POINT('Origin',(-5.55111512312578E-16,5.77350269189626,
10.1599999999987));
#19415=CARTESIAN_POINT('',(-5.,2.88675134594813,10.1599999999987));
#19416=CARTESIAN_POINT('',(-5.,2.88675134594813,10.1599999999987));
#19417=CARTESIAN_POINT('',(-4.,2.3094010767585,9.5826497308091));
#19418=CARTESIAN_POINT('Origin',(-5.,2.88675134594813,10.1599999999987));
#19419=CARTESIAN_POINT('',(-5.00000000000001,-2.88675134594812,10.1599999999987));
#19420=CARTESIAN_POINT('',(-5.,-2.88675134594812,10.1599999999987));
#19421=CARTESIAN_POINT('',(-4.,-2.3094010767585,9.5826497308091));
#19422=CARTESIAN_POINT('Origin',(-5.00000000000001,-2.88675134594812,10.1599999999987));
#19423=CARTESIAN_POINT('',(-1.0547118733939E-14,-5.77350269189626,10.1599999999987));
#19424=CARTESIAN_POINT('',(-6.37301395980167E-15,-5.77350269189625,10.1599999999987));
#19425=CARTESIAN_POINT('',(-4.9960036108132E-15,-4.618802153517,9.5826497308091));
#19426=CARTESIAN_POINT('Origin',(-1.0547118733939E-14,-5.77350269189626,
10.1599999999987));
#19427=CARTESIAN_POINT('',(4.99999999999999,-2.88675134594813,10.1599999999987));
#19428=CARTESIAN_POINT('',(4.99999999999999,-2.88675134594813,10.1599999999987));
#19429=CARTESIAN_POINT('',(4.,-2.3094010767585,9.5826497308091));
#19430=CARTESIAN_POINT('Origin',(4.99999999999999,-2.88675134594813,10.1599999999987));
#19431=CARTESIAN_POINT('',(5.,2.88675134594813,10.1599999999987));
#19432=CARTESIAN_POINT('Origin',(-2.03450935938186E-15,5.77350269189626,
14.9599999999987));
#19433=CARTESIAN_POINT('',(-1.17646633176102E-15,5.77350269189626,14.9599999999987));
#19434=CARTESIAN_POINT('',(5.,2.88675134594813,14.9599999999987));
#19435=CARTESIAN_POINT('',(-4.18000000000003,8.18682681710891,14.9599999999987));
#19436=CARTESIAN_POINT('',(-1.17646633176102E-15,5.77350269189626,14.9599999999987));
#19437=CARTESIAN_POINT('',(5.,2.88675134594813,14.9599999999987));
#19438=CARTESIAN_POINT('Origin',(-5.,2.88675134594813,14.9599999999987));
#19439=CARTESIAN_POINT('',(-5.00000000000001,2.88675134594813,14.9599999999987));
#19440=CARTESIAN_POINT('',(-9.18000000000004,0.473427220735475,14.9599999999987));
#19441=CARTESIAN_POINT('',(-5.00000000000001,2.88675134594813,14.9599999999987));
#19442=CARTESIAN_POINT('Origin',(-5.,-2.88675134594812,14.9599999999987));
#19443=CARTESIAN_POINT('',(-5.00000000000001,-2.88675134594812,14.9599999999987));
#19444=CARTESIAN_POINT('',(-5.,-1.44337567297406,14.9599999999987));
#19445=CARTESIAN_POINT('',(-5.00000000000001,-2.88675134594812,14.9599999999987));
#19446=CARTESIAN_POINT('Origin',(-9.14690518987735E-15,-5.77350269189625,
14.9599999999987));
#19447=CARTESIAN_POINT('',(-1.11684735533874E-14,-5.77350269189626,14.9599999999987));
#19448=CARTESIAN_POINT('',(-6.68000000000004,-1.91680289370953,14.9599999999987));
#19449=CARTESIAN_POINT('',(-1.11684735533874E-14,-5.77350269189626,14.9599999999987));
#19450=CARTESIAN_POINT('Origin',(4.99999999999999,-2.88675134594813,14.9599999999987));
#19451=CARTESIAN_POINT('',(4.99999999999999,-2.88675134594813,14.9599999999987));
#19452=CARTESIAN_POINT('',(-1.68000000000005,-6.74345114413485,14.9599999999987));
#19453=CARTESIAN_POINT('',(4.99999999999999,-2.88675134594813,14.9599999999987));
#19454=CARTESIAN_POINT('Origin',(5.,2.88675134594813,14.9599999999987));
#19455=CARTESIAN_POINT('',(5.,1.44337567297406,14.9599999999987));
#19456=CARTESIAN_POINT('Origin',(-14.4800000000001,0.,14.9599999999987));
#19457=CARTESIAN_POINT('',(14.4799999999999,-1.77328856516537E-15,14.9599999999987));
#19458=CARTESIAN_POINT('Origin',(-8.73577020906364E-14,0.,14.9599999999987));
#19459=CARTESIAN_POINT('Origin',(-8.73388282992177E-14,0.,14.7199999999987));
#19460=CARTESIAN_POINT('',(14.4799999999999,-1.77328856516537E-15,14.7199999999987));
#19461=CARTESIAN_POINT('Origin',(-8.54871728961371E-14,0.,-15.0400000000013));
#19462=CARTESIAN_POINT('',(0.,0.,0.));
#19463=CARTESIAN_POINT('Origin',(-8.50613908013701E-14,0.,-14.2400000000013));
#19464=CARTESIAN_POINT('',(7.91099999999991,9.68818082805471E-16,-13.6663636363649));
#19465=CARTESIAN_POINT('Origin',(-8.5106502022526E-14,0.,-13.6663636363649));
#19466=CARTESIAN_POINT('',(6.39999999999992,-7.83773951454306E-16,-15.0400000000013));
#19467=CARTESIAN_POINT('',(7.27999999999992,8.91542869779273E-16,-14.2400000000013));
#19468=CARTESIAN_POINT('Origin',(-8.4998478163308E-14,0.,-15.0400000000013));
#19469=CARTESIAN_POINT('Origin',(-8.67707890235993E-14,0.,7.49678643762621));
#19470=CARTESIAN_POINT('',(7.91099999999991,9.68818082805471E-16,7.49678643762622));
#19471=CARTESIAN_POINT('Origin',(-8.67707890235993E-14,0.,7.49678643762621));
#19472=CARTESIAN_POINT('',(8.2038932188134,-2.00937431419332E-15,8.20389321881279));
#19473=CARTESIAN_POINT('Origin',(8.91099999999991,-1.09128276272021E-15,
7.49678643762621));
#19474=CARTESIAN_POINT('Origin',(-8.54871728961371E-14,-5.02343578548331E-16,
8.20389321881279));
#19475=CARTESIAN_POINT('Origin',(-8.70651583236477E-14,0.,11.239999999999));
#19476=CARTESIAN_POINT('',(14.4799999999999,-1.77328856516537E-15,14.4799999999987));
#19477=CARTESIAN_POINT('Origin',(-8.73199545077991E-14,0.,14.4799999999987));
#19478=CARTESIAN_POINT('',(11.2399999999999,1.37650300224163E-15,11.239999999999));
#19479=CARTESIAN_POINT('Origin',(-8.59044201514021E-14,0.,-3.52000000000102));
#19480=CARTESIAN_POINT('',(7.91099999999991,-9.68818082805471E-16,-3.52000000000102));
#19481=CARTESIAN_POINT('Origin',(5.,2.88675134594813,10.1599999999987));
#19482=CARTESIAN_POINT('',(5.,2.88675134594813,10.1599999999987));
#19483=CARTESIAN_POINT('',(2.77555756156289E-15,3.60822483003176E-15,7.2732486540506));
#19484=CARTESIAN_POINT('',(3.99999999999999,2.3094010767585,9.5826497308091));
#19485=CARTESIAN_POINT('',(-5.55111512312578E-16,5.77350269189626,10.1599999999987));
#19486=CARTESIAN_POINT('',(-2.13056424354826E-15,5.77350269189626,10.1599999999987));
#19487=CARTESIAN_POINT('',(-1.66533453693773E-15,4.61880215351701,9.5826497308091));
#19488=CARTESIAN_POINT('Origin',(-5.55111512312578E-16,5.77350269189626,
10.1599999999987));
#19489=CARTESIAN_POINT('',(-5.,2.88675134594813,10.1599999999987));
#19490=CARTESIAN_POINT('',(-5.,2.88675134594813,10.1599999999987));
#19491=CARTESIAN_POINT('',(-4.,2.3094010767585,9.5826497308091));
#19492=CARTESIAN_POINT('Origin',(-5.,2.88675134594813,10.1599999999987));
#19493=CARTESIAN_POINT('',(-5.00000000000001,-2.88675134594812,10.1599999999987));
#19494=CARTESIAN_POINT('',(-5.,-2.88675134594812,10.1599999999987));
#19495=CARTESIAN_POINT('',(-4.,-2.3094010767585,9.5826497308091));
#19496=CARTESIAN_POINT('Origin',(-5.00000000000001,-2.88675134594812,10.1599999999987));
#19497=CARTESIAN_POINT('',(-1.0547118733939E-14,-5.77350269189626,10.1599999999987));
#19498=CARTESIAN_POINT('',(-6.37301395980167E-15,-5.77350269189625,10.1599999999987));
#19499=CARTESIAN_POINT('',(-4.9960036108132E-15,-4.618802153517,9.5826497308091));
#19500=CARTESIAN_POINT('Origin',(-1.0547118733939E-14,-5.77350269189626,
10.1599999999987));
#19501=CARTESIAN_POINT('',(4.99999999999999,-2.88675134594813,10.1599999999987));
#19502=CARTESIAN_POINT('',(4.99999999999999,-2.88675134594813,10.1599999999987));
#19503=CARTESIAN_POINT('',(4.,-2.3094010767585,9.5826497308091));
#19504=CARTESIAN_POINT('Origin',(4.99999999999999,-2.88675134594813,10.1599999999987));
#19505=CARTESIAN_POINT('',(5.,2.88675134594813,10.1599999999987));
#19506=CARTESIAN_POINT('Origin',(-2.03450935938186E-15,5.77350269189626,
14.9599999999987));
#19507=CARTESIAN_POINT('',(-1.17646633176102E-15,5.77350269189626,14.9599999999987));
#19508=CARTESIAN_POINT('',(5.,2.88675134594813,14.9599999999987));
#19509=CARTESIAN_POINT('',(-4.18000000000003,8.18682681710891,14.9599999999987));
#19510=CARTESIAN_POINT('',(-1.17646633176102E-15,5.77350269189626,14.9599999999987));
#19511=CARTESIAN_POINT('',(5.,2.88675134594813,14.9599999999987));
#19512=CARTESIAN_POINT('Origin',(-5.,2.88675134594813,14.9599999999987));
#19513=CARTESIAN_POINT('',(-5.00000000000001,2.88675134594813,14.9599999999987));
#19514=CARTESIAN_POINT('',(-9.18000000000004,0.473427220735475,14.9599999999987));
#19515=CARTESIAN_POINT('',(-5.00000000000001,2.88675134594813,14.9599999999987));
#19516=CARTESIAN_POINT('Origin',(-5.,-2.88675134594812,14.9599999999987));
#19517=CARTESIAN_POINT('',(-5.00000000000001,-2.88675134594812,14.9599999999987));
#19518=CARTESIAN_POINT('',(-5.,-1.44337567297406,14.9599999999987));
#19519=CARTESIAN_POINT('',(-5.00000000000001,-2.88675134594812,14.9599999999987));
#19520=CARTESIAN_POINT('Origin',(-9.14690518987735E-15,-5.77350269189625,
14.9599999999987));
#19521=CARTESIAN_POINT('',(-1.11684735533874E-14,-5.77350269189626,14.9599999999987));
#19522=CARTESIAN_POINT('',(-6.68000000000004,-1.91680289370953,14.9599999999987));
#19523=CARTESIAN_POINT('',(-1.11684735533874E-14,-5.77350269189626,14.9599999999987));
#19524=CARTESIAN_POINT('Origin',(4.99999999999999,-2.88675134594813,14.9599999999987));
#19525=CARTESIAN_POINT('',(4.99999999999999,-2.88675134594813,14.9599999999987));
#19526=CARTESIAN_POINT('',(-1.68000000000005,-6.74345114413485,14.9599999999987));
#19527=CARTESIAN_POINT('',(4.99999999999999,-2.88675134594813,14.9599999999987));
#19528=CARTESIAN_POINT('Origin',(5.,2.88675134594813,14.9599999999987));
#19529=CARTESIAN_POINT('',(5.,1.44337567297406,14.9599999999987));
#19530=CARTESIAN_POINT('Origin',(-14.4800000000001,0.,14.9599999999987));
#19531=CARTESIAN_POINT('',(14.4799999999999,-1.77328856516537E-15,14.9599999999987));
#19532=CARTESIAN_POINT('Origin',(-8.73577020906364E-14,0.,14.9599999999987));
#19533=CARTESIAN_POINT('Origin',(-8.73388282992177E-14,0.,14.7199999999987));
#19534=CARTESIAN_POINT('',(14.4799999999999,-1.77328856516537E-15,14.7199999999987));
#19535=CARTESIAN_POINT('Origin',(-8.54871728961371E-14,0.,-15.0400000000013));
#19536=CARTESIAN_POINT('',(0.,0.,0.));
#19537=CARTESIAN_POINT('Origin',(0.,0.,13.));
#19538=CARTESIAN_POINT('',(5.,6.12323399573677E-16,0.));
#19539=CARTESIAN_POINT('Origin',(0.,0.,0.));
#19540=CARTESIAN_POINT('',(5.,6.12323399573677E-16,13.));
#19541=CARTESIAN_POINT('',(5.,-6.12323399573677E-16,13.));
#19542=CARTESIAN_POINT('Origin',(0.,0.,13.));
#19543=CARTESIAN_POINT('Origin',(0.,0.,0.));
#19544=CARTESIAN_POINT('',(-11.,-1.34711147906209E-15,0.));
#19545=CARTESIAN_POINT('Origin',(0.,0.,0.));
#19546=CARTESIAN_POINT('Origin',(0.,0.,-6.72261291411212));
#19547=CARTESIAN_POINT('',(-11.,-1.34711147906209E-15,-6.72261291411212));
#19548=CARTESIAN_POINT('Origin',(0.,0.,-6.72261291411212));
#19549=CARTESIAN_POINT('',(-12.8892103004758,-1.57847301380148E-15,-7.18011159337554));
#19550=CARTESIAN_POINT('Origin',(-12.,-1.46957615897682E-15,-6.72261291411212));
#19551=CARTESIAN_POINT('Origin',(0.,0.,-7.18011159337554));
#19552=CARTESIAN_POINT('Origin',(0.,0.,-3.36130645705606));
#19553=CARTESIAN_POINT('',(-11.,-1.34711147906209E-15,-3.36130645705606));
#19554=CARTESIAN_POINT('Origin',(27.4027293621977,0.,-10.));
#19555=CARTESIAN_POINT('',(-27.4027293621977,-3.35586648013166E-15,-10.));
#19556=CARTESIAN_POINT('Origin',(0.,0.,-10.));
#19557=CARTESIAN_POINT('Origin',(0.,0.,-8.59005579668777));
#19558=CARTESIAN_POINT('',(-27.4027293621977,-3.35586648013166E-15,-7.18011159337554));
#19559=CARTESIAN_POINT('Origin',(0.,0.,-7.18011159337554));
#19560=CARTESIAN_POINT('',(-27.4027293621977,-3.35586648013166E-15,-8.59005579668777));
#19561=CARTESIAN_POINT('Origin',(12.8892103004758,0.,-7.18011159337554));
#19562=CARTESIAN_POINT('Origin',(0.,2.22044604925031E-15,13.));
#19563=CARTESIAN_POINT('',(0.,0.,0.));
#19564=CARTESIAN_POINT('Origin',(0.,0.,-3.5));
#19565=CARTESIAN_POINT('',(-18.2498324643894,-2.234959891249E-15,-2.));
#19566=CARTESIAN_POINT('Origin',(0.,0.,-2.));
#19567=CARTESIAN_POINT('',(-19.7498324643894,-2.4186569111211E-15,-3.5));
#19568=CARTESIAN_POINT('Origin',(-18.2498324643894,-2.23495989124899E-15,
-3.5));
#19569=CARTESIAN_POINT('Origin',(0.,0.,-3.5));
#19570=CARTESIAN_POINT('Origin',(0.,0.,-2.75451686738248));
#19571=CARTESIAN_POINT('',(-19.7498324643894,-2.4186569111211E-15,-3.50903373476496));
#19572=CARTESIAN_POINT('',(-19.7498324643894,-2.4186569111211E-15,-2.75451686738248));
#19573=CARTESIAN_POINT('Origin',(0.,0.,-3.50903373476496));
#19574=CARTESIAN_POINT('Origin',(11.,0.,-2.));
#19575=CARTESIAN_POINT('',(-11.,-1.34711147906209E-15,-2.));
#19576=CARTESIAN_POINT('Origin',(0.,0.,-2.));
#19577=CARTESIAN_POINT('Origin',(0.,0.,-3.5));
#19578=CARTESIAN_POINT('',(-26.6934256722844,-3.26900183078409E-15,-3.5));
#19579=CARTESIAN_POINT('Origin',(0.,0.,-3.5));
#19580=CARTESIAN_POINT('',(-28.1934256722844,-3.45269885065619E-15,-2.));
#19581=CARTESIAN_POINT('Origin',(-28.1934256722844,-3.45269885065619E-15,
-3.5));
#19582=CARTESIAN_POINT('Origin',(0.,0.,-2.));
#19583=CARTESIAN_POINT('Origin',(26.6934256722844,0.,-2.));
#19584=CARTESIAN_POINT('',(-31.5,-3.85763741731416E-15,-2.));
#19585=CARTESIAN_POINT('Origin',(0.,0.,-2.));
#19586=CARTESIAN_POINT('Origin',(0.,0.,-2.75451686738248));
#19587=CARTESIAN_POINT('',(-26.6934256722844,-3.26900183078409E-15,-3.50903373476496));
#19588=CARTESIAN_POINT('Origin',(0.,0.,-3.50903373476496));
#19589=CARTESIAN_POINT('',(-26.6934256722844,-3.26900183078409E-15,-2.75451686738248));
#19590=CARTESIAN_POINT('Origin',(0.,0.,-3.5));
#19591=CARTESIAN_POINT('',(-33.,-4.04133443718627E-15,-3.5));
#19592=CARTESIAN_POINT('Origin',(-31.5,-3.85763741731416E-15,-3.5));
#19593=CARTESIAN_POINT('Origin',(0.,0.,-3.5));
#19594=CARTESIAN_POINT('Origin',(0.,0.,-6.));
#19595=CARTESIAN_POINT('',(-33.,-4.04133443718627E-15,-10.));
#19596=CARTESIAN_POINT('',(-33.,-4.04133443718627E-15,-6.));
#19597=CARTESIAN_POINT('Origin',(0.,0.,-10.));
#19598=CARTESIAN_POINT('Origin',(19.7498324643894,0.,-3.50903373476496));
#19599=CARTESIAN_POINT('Origin',(0.,0.,-4.36130645705606));
#19600=CARTESIAN_POINT('',(-11.,-1.34711147906209E-15,-6.72261291411212));
#19601=CARTESIAN_POINT('Origin',(0.,0.,-6.72261291411212));
#19602=CARTESIAN_POINT('',(-11.,-1.34711147906209E-15,-4.36130645705606));
#19603=CARTESIAN_POINT('Origin',(0.,0.,-6.72261291411212));
#19604=CARTESIAN_POINT('',(-12.8892103004758,-1.57847301380148E-15,-7.18011159337554));
#19605=CARTESIAN_POINT('Origin',(0.,0.,-7.18011159337554));
#19606=CARTESIAN_POINT('Origin',(-12.,-1.46957615897682E-15,-6.72261291411212));
#19607=CARTESIAN_POINT('Origin',(27.4027293621977,0.,-7.18011159337554));
#19608=CARTESIAN_POINT('',(-27.4027293621977,-3.35586648013166E-15,-7.18011159337554));
#19609=CARTESIAN_POINT('Origin',(0.,0.,-7.18011159337554));
#19610=CARTESIAN_POINT('Origin',(0.,0.,-6.42664169815681));
#19611=CARTESIAN_POINT('',(-27.4027293621977,-3.35586648013166E-15,-5.67317180293808));
#19612=CARTESIAN_POINT('Origin',(0.,0.,-5.67317180293808));
#19613=CARTESIAN_POINT('',(-27.4027293621977,-3.35586648013166E-15,-6.42664169815681));
#19614=CARTESIAN_POINT('Origin',(29.0578798664922,0.,-5.67317180293808));
#19615=CARTESIAN_POINT('',(-29.0578798664922,-3.5585639568508E-15,-5.67317180293808));
#19616=CARTESIAN_POINT('Origin',(0.,0.,-5.67317180293808));
#19617=CARTESIAN_POINT('Origin',(0.,0.,-6.42664169815681));
#19618=CARTESIAN_POINT('',(-29.0578798664922,-3.5585639568508E-15,-7.18011159337554));
#19619=CARTESIAN_POINT('Origin',(0.,0.,-7.18011159337554));
#19620=CARTESIAN_POINT('',(-29.0578798664922,-3.5585639568508E-15,-6.42664169815681));
#19621=CARTESIAN_POINT('Origin',(31.1192710879259,0.,-7.18011159337554));
#19622=CARTESIAN_POINT('',(-31.1192710879259,-3.81101157296272E-15,-7.18011159337554));
#19623=CARTESIAN_POINT('Origin',(0.,0.,-7.18011159337554));
#19624=CARTESIAN_POINT('Origin',(0.,0.,-8.59005579668777));
#19625=CARTESIAN_POINT('',(-31.1192710879259,-3.81101157296272E-15,-10.));
#19626=CARTESIAN_POINT('Origin',(0.,0.,-10.));
#19627=CARTESIAN_POINT('',(-31.1192710879259,-3.81101157296272E-15,-8.59005579668777));
#19628=CARTESIAN_POINT('Origin',(33.,0.,-10.));
#19629=CARTESIAN_POINT('',(0.,0.,0.));
#19630=CARTESIAN_POINT('Origin',(31.8615483148624,-24.,0.));
#19631=CARTESIAN_POINT('',(31.062799572083,-23.3983352711781,-6.));
#19632=CARTESIAN_POINT('',(31.8615483148624,-25.,-6.));
#19633=CARTESIAN_POINT('Origin',(31.8615483148624,-24.,-6.));
#19634=CARTESIAN_POINT('',(31.062799572083,-23.3983352711781,-10.));
#19635=CARTESIAN_POINT('',(31.062799572083,-23.3983352711781,0.));
#19636=CARTESIAN_POINT('',(31.8615483148624,-25.,-10.));
#19637=CARTESIAN_POINT('Origin',(31.8615483148624,-24.,-10.));
#19638=CARTESIAN_POINT('',(31.8615483148624,-25.,0.));
#19639=CARTESIAN_POINT('Origin',(0.,0.,-6.));
#19640=CARTESIAN_POINT('',(31.062799572083,23.3983352711781,-6.));
#19641=CARTESIAN_POINT('',(31.8615483148624,24.,-5.));
#19642=CARTESIAN_POINT('Origin',(31.8615483148624,24.,-6.));
#19643=CARTESIAN_POINT('Origin',(0.,0.,-6.));
#19644=CARTESIAN_POINT('',(31.8615483148624,-24.,-5.));
#19645=CARTESIAN_POINT('Origin',(31.8615483148624,-24.,-6.));
#19646=CARTESIAN_POINT('Origin',(0.,0.,-5.));
#19647=CARTESIAN_POINT('Origin',(31.8615483148624,-24.,-6.));
#19648=CARTESIAN_POINT('Origin',(31.8615483148624,-24.,-6.));
#19649=CARTESIAN_POINT('Origin',(31.8615483148624,24.,0.));
#19650=CARTESIAN_POINT('',(31.8615483148624,25.,-6.));
#19651=CARTESIAN_POINT('Origin',(31.8615483148624,24.,-6.));
#19652=CARTESIAN_POINT('',(31.8615483148624,25.,-10.));
#19653=CARTESIAN_POINT('',(31.8615483148624,25.,0.));
#19654=CARTESIAN_POINT('',(31.062799572083,23.3983352711781,-10.));
#19655=CARTESIAN_POINT('Origin',(31.8615483148624,24.,-10.));
#19656=CARTESIAN_POINT('',(31.062799572083,23.3983352711781,0.));
#19657=CARTESIAN_POINT('Origin',(31.8615483148624,24.,-6.));
#19658=CARTESIAN_POINT('Origin',(31.8615483148624,24.,-6.));
#19659=CARTESIAN_POINT('Origin',(29.7889175821791,-25.,0.));
#19660=CARTESIAN_POINT('',(21.540659228538,-25.,-10.));
#19661=CARTESIAN_POINT('',(25.8778257092103,-25.,-10.));
#19662=CARTESIAN_POINT('',(21.540659228538,-25.,-14.));
#19663=CARTESIAN_POINT('',(21.540659228538,-25.,-11.));
#19664=CARTESIAN_POINT('',(70.,-25.,-14.));
#19665=CARTESIAN_POINT('',(75.,-25.,-14.));
#19666=CARTESIAN_POINT('',(70.,-25.,-6.));
#19667=CARTESIAN_POINT('',(70.,-25.,0.));
#19668=CARTESIAN_POINT('',(41.0916881866343,-25.,-6.));
#19669=CARTESIAN_POINT('Origin',(41.0916881866343,-24.,-6.));
#19670=CARTESIAN_POINT('',(70.,-24.,-5.));
#19671=CARTESIAN_POINT('Origin',(70.,-24.,-6.));
#19672=CARTESIAN_POINT('',(41.0916881866343,-24.,-5.));
#19673=CARTESIAN_POINT('Origin',(52.3944587910896,0.,-5.));
#19674=CARTESIAN_POINT('',(74.,-20.,-5.));
#19675=CARTESIAN_POINT('Origin',(70.,-20.,-5.));
#19676=CARTESIAN_POINT('',(74.,20.,-5.));
#19677=CARTESIAN_POINT('',(74.,-12.5,-5.));
#19678=CARTESIAN_POINT('',(70.,24.,-5.));
#19679=CARTESIAN_POINT('Origin',(70.,20.,-5.));
#19680=CARTESIAN_POINT('',(63.6972293955448,24.,-5.));
#19681=CARTESIAN_POINT('',(71.5444185458617,-1.3259677713873E-15,-5.));
#19682=CARTESIAN_POINT('Origin',(60.7170700212872,0.,-5.));
#19683=CARTESIAN_POINT('Origin',(63.6972293955448,24.,-6.));
#19684=CARTESIAN_POINT('',(70.,25.,-6.));
#19685=CARTESIAN_POINT('Origin',(70.,24.,-6.));
#19686=CARTESIAN_POINT('',(63.6972293955448,25.,-6.));
#19687=CARTESIAN_POINT('Origin',(75.,25.,0.));
#19688=CARTESIAN_POINT('',(70.,25.,-14.));
#19689=CARTESIAN_POINT('',(70.,25.,0.));
#19690=CARTESIAN_POINT('',(21.540659228538,25.,-14.));
#19691=CARTESIAN_POINT('',(-75.,25.,-14.));
#19692=CARTESIAN_POINT('',(21.540659228538,25.,-10.));
#19693=CARTESIAN_POINT('',(21.540659228538,25.,-11.));
#19694=CARTESIAN_POINT('',(30.0019548860308,25.,-10.));
#19695=CARTESIAN_POINT('Origin',(70.,-20.,-6.));
#19696=CARTESIAN_POINT('',(75.,-20.,-6.));
#19697=CARTESIAN_POINT('Origin',(74.,-20.,-6.));
#19698=CARTESIAN_POINT('Origin',(70.,-20.,-6.));
#19699=CARTESIAN_POINT('Origin',(74.,-12.5,-6.));
#19700=CARTESIAN_POINT('',(75.,20.,-6.));
#19701=CARTESIAN_POINT('Origin',(74.,20.,-6.));
#19702=CARTESIAN_POINT('',(75.,-12.5,-6.));
#19703=CARTESIAN_POINT('Origin',(70.,20.,-6.));
#19704=CARTESIAN_POINT('Origin',(70.,20.,-6.));
#19705=CARTESIAN_POINT('Origin',(60.7170700212872,0.,-6.));
#19706=CARTESIAN_POINT('',(69.5444185458617,1.08103841155783E-15,-7.));
#19707=CARTESIAN_POINT('Origin',(60.7170700212872,0.,-7.));
#19708=CARTESIAN_POINT('',(70.5444185458617,1.20350309147256E-15,-6.));
#19709=CARTESIAN_POINT('Origin',(60.7170700212872,0.,0.));
#19710=CARTESIAN_POINT('',(69.5444185458617,-1.08103841155783E-15,-14.));
#19711=CARTESIAN_POINT('Origin',(60.7170700212872,0.,-14.));
#19712=CARTESIAN_POINT('',(69.5444185458617,1.08103841155783E-15,0.));
#19713=CARTESIAN_POINT('Origin',(70.,-20.,0.));
#19714=CARTESIAN_POINT('',(75.,-20.,-14.));
#19715=CARTESIAN_POINT('Origin',(70.,-20.,-14.));
#19716=CARTESIAN_POINT('',(75.,-20.,0.));
#19717=CARTESIAN_POINT('Origin',(75.,-25.,0.));
#19718=CARTESIAN_POINT('',(75.,20.,-14.));
#19719=CARTESIAN_POINT('',(75.,25.,-14.));
#19720=CARTESIAN_POINT('',(75.,20.,0.));
#19721=CARTESIAN_POINT('Origin',(70.,20.,0.));
#19722=CARTESIAN_POINT('Origin',(70.,20.,-14.));
#19723=CARTESIAN_POINT('Origin',(0.,0.,0.));
#19724=CARTESIAN_POINT('Origin',(0.,0.,-10.));
#19725=CARTESIAN_POINT('Origin',(0.,0.,-11.));
#19726=CARTESIAN_POINT('',(-21.540659228538,25.,-14.));
#19727=CARTESIAN_POINT('Origin',(0.,0.,-14.));
#19728=CARTESIAN_POINT('',(-21.540659228538,25.,-10.));
#19729=CARTESIAN_POINT('',(-21.540659228538,25.,-11.));
#19730=CARTESIAN_POINT('Origin',(0.,0.,-10.));
#19731=CARTESIAN_POINT('Origin',(0.,0.,-11.));
#19732=CARTESIAN_POINT('',(-21.540659228538,-25.,-10.));
#19733=CARTESIAN_POINT('Origin',(0.,0.,-10.));
#19734=CARTESIAN_POINT('',(-21.540659228538,-25.,-14.));
#19735=CARTESIAN_POINT('',(-21.540659228538,-25.,-11.));
#19736=CARTESIAN_POINT('Origin',(0.,0.,-14.));
#19737=CARTESIAN_POINT('Origin',(-31.8615483148624,-24.,0.));
#19738=CARTESIAN_POINT('',(-31.062799572083,-23.3983352711781,-6.));
#19739=CARTESIAN_POINT('',(-31.8615483148624,-25.,-6.));
#19740=CARTESIAN_POINT('Origin',(-31.8615483148624,-24.,-6.));
#19741=CARTESIAN_POINT('',(-31.8615483148624,-25.,-10.));
#19742=CARTESIAN_POINT('',(-31.8615483148624,-25.,0.));
#19743=CARTESIAN_POINT('',(-31.062799572083,-23.3983352711781,-10.));
#19744=CARTESIAN_POINT('Origin',(-31.8615483148624,-24.,-10.));
#19745=CARTESIAN_POINT('',(-31.062799572083,-23.3983352711781,0.));
#19746=CARTESIAN_POINT('Origin',(0.,0.,-6.));
#19747=CARTESIAN_POINT('',(-31.062799572083,23.3983352711781,-6.));
#19748=CARTESIAN_POINT('',(-31.8615483148624,24.,-5.));
#19749=CARTESIAN_POINT('Origin',(-31.8615483148624,24.,-6.));
#19750=CARTESIAN_POINT('',(-31.8615483148624,-24.,-5.));
#19751=CARTESIAN_POINT('Origin',(0.,0.,-5.));
#19752=CARTESIAN_POINT('Origin',(-31.8615483148624,-24.,-6.));
#19753=CARTESIAN_POINT('Origin',(0.,0.,-6.));
#19754=CARTESIAN_POINT('Origin',(-31.8615483148624,-24.,-6.));
#19755=CARTESIAN_POINT('Origin',(-31.8615483148624,-24.,-6.));
#19756=CARTESIAN_POINT('Origin',(-31.8615483148624,24.,0.));
#19757=CARTESIAN_POINT('',(-31.8615483148624,25.,-6.));
#19758=CARTESIAN_POINT('Origin',(-31.8615483148624,24.,-6.));
#19759=CARTESIAN_POINT('',(-31.062799572083,23.3983352711781,-10.));
#19760=CARTESIAN_POINT('',(-31.062799572083,23.3983352711781,0.));
#19761=CARTESIAN_POINT('',(-31.8615483148624,25.,-10.));
#19762=CARTESIAN_POINT('Origin',(-31.8615483148624,24.,-10.));
#19763=CARTESIAN_POINT('',(-31.8615483148624,25.,0.));
#19764=CARTESIAN_POINT('Origin',(-31.8615483148624,24.,-6.));
#19765=CARTESIAN_POINT('Origin',(-31.8615483148624,24.,-6.));
#19766=CARTESIAN_POINT('Origin',(-29.7889175821791,-25.,0.));
#19767=CARTESIAN_POINT('',(-25.8778257092103,-25.,-10.));
#19768=CARTESIAN_POINT('',(-70.,-25.,-6.));
#19769=CARTESIAN_POINT('',(-41.0916881866343,-25.,-6.));
#19770=CARTESIAN_POINT('',(-70.,-25.,-14.));
#19771=CARTESIAN_POINT('',(-70.,-25.,0.));
#19772=CARTESIAN_POINT('',(-75.,-25.,-14.));
#19773=CARTESIAN_POINT('Origin',(-41.0916881866343,-24.,-6.));
#19774=CARTESIAN_POINT('',(-70.,-24.,-5.));
#19775=CARTESIAN_POINT('',(-41.0916881866343,-24.,-5.));
#19776=CARTESIAN_POINT('Origin',(-70.,-24.,-6.));
#19777=CARTESIAN_POINT('Origin',(-52.3944587910896,0.,-5.));
#19778=CARTESIAN_POINT('',(-70.,24.,-5.));
#19779=CARTESIAN_POINT('',(-63.6972293955448,24.,-5.));
#19780=CARTESIAN_POINT('',(-74.,20.,-5.));
#19781=CARTESIAN_POINT('Origin',(-70.,20.,-5.));
#19782=CARTESIAN_POINT('',(-74.,-20.,-5.));
#19783=CARTESIAN_POINT('',(-74.,-12.5,-5.));
#19784=CARTESIAN_POINT('Origin',(-70.,-20.,-5.));
#19785=CARTESIAN_POINT('',(-71.5444185458617,-1.3259677713873E-15,-5.));
#19786=CARTESIAN_POINT('Origin',(-60.7170700212872,0.,-5.));
#19787=CARTESIAN_POINT('Origin',(-63.6972293955448,24.,-6.));
#19788=CARTESIAN_POINT('',(-70.,25.,-6.));
#19789=CARTESIAN_POINT('',(-63.6972293955448,25.,-6.));
#19790=CARTESIAN_POINT('Origin',(-70.,24.,-6.));
#19791=CARTESIAN_POINT('Origin',(-75.,25.,0.));
#19792=CARTESIAN_POINT('',(-30.0019548860308,25.,-10.));
#19793=CARTESIAN_POINT('',(-70.,25.,-14.));
#19794=CARTESIAN_POINT('',(75.,25.,-14.));
#19795=CARTESIAN_POINT('',(-70.,25.,0.));
#19796=CARTESIAN_POINT('Origin',(-70.,-20.,-6.));
#19797=CARTESIAN_POINT('',(-75.,-20.,-6.));
#19798=CARTESIAN_POINT('Origin',(-74.,-20.,-6.));
#19799=CARTESIAN_POINT('Origin',(-70.,-20.,-6.));
#19800=CARTESIAN_POINT('Origin',(-74.,-12.5,-6.));
#19801=CARTESIAN_POINT('',(-75.,20.,-6.));
#19802=CARTESIAN_POINT('Origin',(-74.,20.,-6.));
#19803=CARTESIAN_POINT('',(-75.,-12.5,-6.));
#19804=CARTESIAN_POINT('Origin',(-70.,20.,-6.));
#19805=CARTESIAN_POINT('Origin',(-70.,20.,-6.));
#19806=CARTESIAN_POINT('Origin',(-60.7170700212872,0.,-6.));
#19807=CARTESIAN_POINT('',(-69.5444185458617,1.08103841155783E-15,-7.));
#19808=CARTESIAN_POINT('Origin',(-60.7170700212872,0.,-7.));
#19809=CARTESIAN_POINT('',(-70.5444185458617,-1.20350309147256E-15,-6.));
#19810=CARTESIAN_POINT('Origin',(-60.7170700212872,0.,0.));
#19811=CARTESIAN_POINT('',(-69.5444185458617,-1.08103841155783E-15,-14.));
#19812=CARTESIAN_POINT('',(-69.5444185458617,1.08103841155783E-15,0.));
#19813=CARTESIAN_POINT('Origin',(-60.7170700212872,0.,-14.));
#19814=CARTESIAN_POINT('Origin',(-70.,-20.,0.));
#19815=CARTESIAN_POINT('',(-75.,-20.,-14.));
#19816=CARTESIAN_POINT('',(-75.,-20.,0.));
#19817=CARTESIAN_POINT('Origin',(-70.,-20.,-14.));
#19818=CARTESIAN_POINT('Origin',(-75.,-25.,0.));
#19819=CARTESIAN_POINT('',(-75.,20.,-14.));
#19820=CARTESIAN_POINT('',(-75.,20.,0.));
#19821=CARTESIAN_POINT('',(-75.,25.,-14.));
#19822=CARTESIAN_POINT('Origin',(-70.,20.,0.));
#19823=CARTESIAN_POINT('Origin',(-70.,20.,-14.));
#19824=CARTESIAN_POINT('Origin',(0.,0.,0.));
#19825=CARTESIAN_POINT('Origin',(0.,0.,-10.));
#19826=CARTESIAN_POINT('Origin',(0.,0.,-7.83658590146904));
#19827=CARTESIAN_POINT('',(-27.4027293621977,-3.35586648013166E-15,-10.));
#19828=CARTESIAN_POINT('Origin',(0.,0.,-10.));
#19829=CARTESIAN_POINT('',(-27.4027293621977,-3.35586648013166E-15,-5.67317180293808));
#19830=CARTESIAN_POINT('',(-27.4027293621977,-3.35586648013166E-15,-7.83658590146904));
#19831=CARTESIAN_POINT('Origin',(0.,0.,-5.67317180293808));
#19832=CARTESIAN_POINT('Origin',(0.,0.,-10.));
#19833=CARTESIAN_POINT('Origin',(33.,0.,-14.));
#19834=CARTESIAN_POINT('Origin',(31.1192710879259,0.,-10.));
#19835=CARTESIAN_POINT('',(-31.1192710879259,-3.81101157296272E-15,-10.));
#19836=CARTESIAN_POINT('Origin',(0.,0.,-10.));
#19837=CARTESIAN_POINT('Origin',(0.,0.,-8.59005579668777));
#19838=CARTESIAN_POINT('',(-31.1192710879259,-3.81101157296272E-15,-7.18011159337554));
#19839=CARTESIAN_POINT('Origin',(0.,0.,-7.18011159337554));
#19840=CARTESIAN_POINT('',(-31.1192710879259,-3.81101157296272E-15,-8.59005579668777));
#19841=CARTESIAN_POINT('Origin',(29.0578798664922,0.,-7.18011159337554));
#19842=CARTESIAN_POINT('',(-29.0578798664922,-3.5585639568508E-15,-7.18011159337554));
#19843=CARTESIAN_POINT('Origin',(0.,0.,-7.18011159337554));
#19844=CARTESIAN_POINT('Origin',(0.,0.,-6.42664169815681));
#19845=CARTESIAN_POINT('',(-29.0578798664922,-3.5585639568508E-15,-5.67317180293808));
#19846=CARTESIAN_POINT('Origin',(0.,0.,-5.67317180293808));
#19847=CARTESIAN_POINT('',(-29.0578798664922,-3.5585639568508E-15,-6.42664169815681));
#19848=CARTESIAN_POINT('Origin',(27.4027293621977,0.,-5.67317180293808));
#19849=CARTESIAN_POINT('',(0.,0.,0.));
#19850=CARTESIAN_POINT('Origin',(0.,0.,-6.72261291411212));
#19851=CARTESIAN_POINT('',(-11.,-1.34711147906209E-15,-6.72261291411212));
#19852=CARTESIAN_POINT('Origin',(-12.,-1.46957615897682E-15,-6.72261291411212));
#19853=CARTESIAN_POINT('Origin',(0.,0.,-6.72261291411212));
#19854=CARTESIAN_POINT('',(0.,0.,0.));
#19855=CARTESIAN_POINT('',(-60.7170700212872,0.,-15.8273485245745));
#19856=CARTESIAN_POINT('',(60.7170700212872,0.,-15.8273485245745));
#19857=CARTESIAN_POINT('',(0.,0.,0.));
#19858=CARTESIAN_POINT('',(0.,0.,0.));
#19859=CARTESIAN_POINT('',(0.,0.,0.));
#19860=CARTESIAN_POINT('',(0.,0.,0.));
#19861=UNCERTAINTY_MEASURE_WITH_UNIT(LENGTH_MEASURE(0.01),#19879,
'DISTANCE_ACCURACY_VALUE',
'Maximum model space distance between geometric entities at asserted c
onnectivities');
#19862=UNCERTAINTY_MEASURE_WITH_UNIT(LENGTH_MEASURE(0.01),#19879,
'DISTANCE_ACCURACY_VALUE',
'Maximum model space distance between geometric entities at asserted c
onnectivities');
#19863=UNCERTAINTY_MEASURE_WITH_UNIT(LENGTH_MEASURE(0.01),#19879,
'DISTANCE_ACCURACY_VALUE',
'Maximum model space distance between geometric entities at asserted c
onnectivities');
#19864=UNCERTAINTY_MEASURE_WITH_UNIT(LENGTH_MEASURE(0.01),#19879,
'DISTANCE_ACCURACY_VALUE',
'Maximum model space distance between geometric entities at asserted c
onnectivities');
#19865=UNCERTAINTY_MEASURE_WITH_UNIT(LENGTH_MEASURE(0.01),#19879,
'DISTANCE_ACCURACY_VALUE',
'Maximum model space distance between geometric entities at asserted c
onnectivities');
#19866=UNCERTAINTY_MEASURE_WITH_UNIT(LENGTH_MEASURE(0.01),#19879,
'DISTANCE_ACCURACY_VALUE',
'Maximum model space distance between geometric entities at asserted c
onnectivities');
#19867=UNCERTAINTY_MEASURE_WITH_UNIT(LENGTH_MEASURE(0.01),#19879,
'DISTANCE_ACCURACY_VALUE',
'Maximum model space distance between geometric entities at asserted c
onnectivities');
#19868=UNCERTAINTY_MEASURE_WITH_UNIT(LENGTH_MEASURE(0.01),#19879,
'DISTANCE_ACCURACY_VALUE',
'Maximum model space distance between geometric entities at asserted c
onnectivities');
#19869=UNCERTAINTY_MEASURE_WITH_UNIT(LENGTH_MEASURE(0.01),#19879,
'DISTANCE_ACCURACY_VALUE',
'Maximum model space distance between geometric entities at asserted c
onnectivities');
#19870=(
GEOMETRIC_REPRESENTATION_CONTEXT(3)
GLOBAL_UNCERTAINTY_ASSIGNED_CONTEXT((#19861))
GLOBAL_UNIT_ASSIGNED_CONTEXT((#19879,#19881,#19882))
REPRESENTATION_CONTEXT('','3D')
);
#19871=(
GEOMETRIC_REPRESENTATION_CONTEXT(3)
GLOBAL_UNCERTAINTY_ASSIGNED_CONTEXT((#19862))
GLOBAL_UNIT_ASSIGNED_CONTEXT((#19879,#19881,#19882))
REPRESENTATION_CONTEXT('','3D')
);
#19872=(
GEOMETRIC_REPRESENTATION_CONTEXT(3)
GLOBAL_UNCERTAINTY_ASSIGNED_CONTEXT((#19863))
GLOBAL_UNIT_ASSIGNED_CONTEXT((#19879,#19881,#19882))
REPRESENTATION_CONTEXT('','3D')
);
#19873=(
GEOMETRIC_REPRESENTATION_CONTEXT(3)
GLOBAL_UNCERTAINTY_ASSIGNED_CONTEXT((#19864))
GLOBAL_UNIT_ASSIGNED_CONTEXT((#19879,#19881,#19882))
REPRESENTATION_CONTEXT('','3D')
);
#19874=(
GEOMETRIC_REPRESENTATION_CONTEXT(3)
GLOBAL_UNCERTAINTY_ASSIGNED_CONTEXT((#19865))
GLOBAL_UNIT_ASSIGNED_CONTEXT((#19879,#19881,#19882))
REPRESENTATION_CONTEXT('','3D')
);
#19875=(
GEOMETRIC_REPRESENTATION_CONTEXT(3)
GLOBAL_UNCERTAINTY_ASSIGNED_CONTEXT((#19866))
GLOBAL_UNIT_ASSIGNED_CONTEXT((#19879,#19881,#19882))
REPRESENTATION_CONTEXT('','3D')
);
#19876=(
GEOMETRIC_REPRESENTATION_CONTEXT(3)
GLOBAL_UNCERTAINTY_ASSIGNED_CONTEXT((#19867))
GLOBAL_UNIT_ASSIGNED_CONTEXT((#19879,#19881,#19882))
REPRESENTATION_CONTEXT('','3D')
);
#19877=(
GEOMETRIC_REPRESENTATION_CONTEXT(3)
GLOBAL_UNCERTAINTY_ASSIGNED_CONTEXT((#19868))
GLOBAL_UNIT_ASSIGNED_CONTEXT((#19879,#19881,#19882))
REPRESENTATION_CONTEXT('','3D')
);
#19878=(
GEOMETRIC_REPRESENTATION_CONTEXT(3)
GLOBAL_UNCERTAINTY_ASSIGNED_CONTEXT((#19869))
GLOBAL_UNIT_ASSIGNED_CONTEXT((#19879,#19881,#19882))
REPRESENTATION_CONTEXT('','3D')
);
#19879=(
LENGTH_UNIT()
NAMED_UNIT(*)
SI_UNIT(.MILLI.,.METRE.)
);
#19880=(
LENGTH_UNIT()
NAMED_UNIT(*)
SI_UNIT($,.METRE.)
);
#19881=(
NAMED_UNIT(*)
PLANE_ANGLE_UNIT()
SI_UNIT($,.RADIAN.)
);
#19882=(
NAMED_UNIT(*)
SI_UNIT($,.STERADIAN.)
SOLID_ANGLE_UNIT()
);
#19883=SHAPE_DEFINITION_REPRESENTATION(#19891,#19906);
#19884=SHAPE_DEFINITION_REPRESENTATION(#19892,#19907);
#19885=SHAPE_DEFINITION_REPRESENTATION(#19893,#19908);
#19886=SHAPE_DEFINITION_REPRESENTATION(#19894,#19909);
#19887=SHAPE_DEFINITION_REPRESENTATION(#19895,#19910);
#19888=SHAPE_DEFINITION_REPRESENTATION(#19896,#19911);
#19889=SHAPE_DEFINITION_REPRESENTATION(#19897,#19912);
#19890=SHAPE_DEFINITION_REPRESENTATION(#19898,#19913);
#19891=PRODUCT_DEFINITION_SHAPE('',$,#19915);
#19892=PRODUCT_DEFINITION_SHAPE('',$,#19916);
#19893=PRODUCT_DEFINITION_SHAPE('',$,#19917);
#19894=PRODUCT_DEFINITION_SHAPE('',$,#19918);
#19895=PRODUCT_DEFINITION_SHAPE('',$,#19919);
#19896=PRODUCT_DEFINITION_SHAPE('',$,#19920);
#19897=PRODUCT_DEFINITION_SHAPE('',$,#19921);
#19898=PRODUCT_DEFINITION_SHAPE('',$,#19922);
#19899=PRODUCT_DEFINITION_SHAPE($,$,#32);
#19900=PRODUCT_DEFINITION_SHAPE($,$,#33);
#19901=PRODUCT_DEFINITION_SHAPE($,$,#34);
#19902=PRODUCT_DEFINITION_SHAPE($,$,#35);
#19903=PRODUCT_DEFINITION_SHAPE($,$,#36);
#19904=PRODUCT_DEFINITION_SHAPE($,$,#37);
#19905=PRODUCT_DEFINITION_SHAPE($,$,#38);
#19906=SHAPE_REPRESENTATION('',(#4910,#5420,#5421,#5422,#5423,#5424,#5425,
#5426),#19870);
#19907=SHAPE_REPRESENTATION('',(#4911),#19871);
#19908=SHAPE_REPRESENTATION('',(#5197),#19872);
#19909=SHAPE_REPRESENTATION('',(#5224),#19873);
#19910=SHAPE_REPRESENTATION('',(#5251),#19874);
#19911=SHAPE_REPRESENTATION('',(#5268),#19875);
#19912=SHAPE_REPRESENTATION('',(#5309),#19876);
#19913=SHAPE_REPRESENTATION('',(#5416),#19877);
#19914=PRODUCT_DEFINITION_CONTEXT('part definition',#19940,'design');
#19915=PRODUCT_DEFINITION('BR-110','BR-110',#19923,#19914);
#19916=PRODUCT_DEFINITION('Gear','Gear',#19924,#19914);
#19917=PRODUCT_DEFINITION(
'BHSFCHCS ANSI B18.3.5M - M16x30 Steel Grade 2 Plain','Screw_02',#19925,
#19914);
#19918=PRODUCT_DEFINITION(
'BHSFCHCS ANSI B18.3.5M - M16x30 Steel Grade 2 Plain_1','Screw_01',#19926,
#19914);
#19919=PRODUCT_DEFINITION('Rotor','Rotor',#19927,#19914);
#19920=PRODUCT_DEFINITION('Disc','Disc',#19928,#19914);
#19921=PRODUCT_DEFINITION('base','Base',#19929,#19914);
#19922=PRODUCT_DEFINITION('O_Ring','O_Ring',#19930,#19914);
#19923=PRODUCT_DEFINITION_FORMATION('',$,#19942);
#19924=PRODUCT_DEFINITION_FORMATION('',$,#19943);
#19925=PRODUCT_DEFINITION_FORMATION('',$,#19944);
#19926=PRODUCT_DEFINITION_FORMATION('',$,#19945);
#19927=PRODUCT_DEFINITION_FORMATION('',$,#19946);
#19928=PRODUCT_DEFINITION_FORMATION('',$,#19947);
#19929=PRODUCT_DEFINITION_FORMATION('',$,#19948);
#19930=PRODUCT_DEFINITION_FORMATION('',$,#19949);
#19931=PRODUCT_RELATED_PRODUCT_CATEGORY('BR-110','BR-110',(#19942));
#19932=PRODUCT_RELATED_PRODUCT_CATEGORY('Gear','Gear',(#19943));
#19933=PRODUCT_RELATED_PRODUCT_CATEGORY('Screw_02','Screw_02',(#19944));
#19934=PRODUCT_RELATED_PRODUCT_CATEGORY('Screw_01','Screw_01',(#19945));
#19935=PRODUCT_RELATED_PRODUCT_CATEGORY('Rotor','Rotor',(#19946));
#19936=PRODUCT_RELATED_PRODUCT_CATEGORY('Disc','Disc',(#19947));
#19937=PRODUCT_RELATED_PRODUCT_CATEGORY('Base','Base',(#19948));
#19938=PRODUCT_RELATED_PRODUCT_CATEGORY('O_Ring','O_Ring',(#19949));
#19939=APPLICATION_PROTOCOL_DEFINITION('international standard',
'automotive_design',2009,#19940);
#19940=APPLICATION_CONTEXT(
'Core Data for Automotive Mechanical Design Process');
#19941=PRODUCT_CONTEXT('part definition',#19940,'mechanical');
#19942=PRODUCT('BR-110','BR-110',$,(#19941));
#19943=PRODUCT('Gear','Gear',
'Spur Gear; Module: 2.0; Num Teeth: 20; Pressure Angle: 20.0; Backlash
: 0.00 mm',(#19941));
#19944=PRODUCT('BHSFCHCS ANSI B18.3.5M - M16x30 Steel Grade 2 Plain',
'Screw_02',
'Broached Hexagon Socket Flat Countersunk Head Cap Screw ANSI B18.3.5M
 - M16x30',(#19941));
#19945=PRODUCT('BHSFCHCS ANSI B18.3.5M - M16x30 Steel Grade 2 Plain_1',
'Screw_01',
'Broached Hexagon Socket Flat Countersunk Head Cap Screw ANSI B18.3.5M
 - M16x30',(#19941));
#19946=PRODUCT('Rotor','Rotor',$,(#19941));
#19947=PRODUCT('Disc','Disc',$,(#19941));
#19948=PRODUCT('base','Base',$,(#19941));
#19949=PRODUCT('O_Ring','O_Ring',$,(#19941));
#19950=PRESENTATION_STYLE_ASSIGNMENT((#19956));
#19951=PRESENTATION_STYLE_ASSIGNMENT((#19957));
#19952=PRESENTATION_STYLE_ASSIGNMENT((#19958));
#19953=PRESENTATION_STYLE_ASSIGNMENT((#19959));
#19954=PRESENTATION_STYLE_ASSIGNMENT((#19960));
#19955=PRESENTATION_STYLE_ASSIGNMENT((#19961));
#19956=SURFACE_STYLE_USAGE(.BOTH.,#19962);
#19957=SURFACE_STYLE_USAGE(.BOTH.,#19963);
#19958=SURFACE_STYLE_USAGE(.BOTH.,#19964);
#19959=SURFACE_STYLE_USAGE(.BOTH.,#19965);
#19960=SURFACE_STYLE_USAGE(.BOTH.,#19966);
#19961=SURFACE_STYLE_USAGE(.BOTH.,#19967);
#19962=SURFACE_SIDE_STYLE('',(#19968));
#19963=SURFACE_SIDE_STYLE('',(#19969));
#19964=SURFACE_SIDE_STYLE('',(#19970));
#19965=SURFACE_SIDE_STYLE('',(#19971));
#19966=SURFACE_SIDE_STYLE('',(#19972));
#19967=SURFACE_SIDE_STYLE('',(#19973));
#19968=SURFACE_STYLE_FILL_AREA(#19974);
#19969=SURFACE_STYLE_FILL_AREA(#19975);
#19970=SURFACE_STYLE_FILL_AREA(#19976);
#19971=SURFACE_STYLE_FILL_AREA(#19977);
#19972=SURFACE_STYLE_FILL_AREA(#19978);
#19973=SURFACE_STYLE_FILL_AREA(#19979);
#19974=FILL_AREA_STYLE('Steel - Satin',(#19980));
#19975=FILL_AREA_STYLE('Opaque(203,203,203)',(#19981));
#19976=FILL_AREA_STYLE('Opaque(160,160,160)',(#19982));
#19977=FILL_AREA_STYLE('Opaque(255,85,127)',(#19983));
#19978=FILL_AREA_STYLE('Opaque(170,0,255)',(#19984));
#19979=FILL_AREA_STYLE('Opaque(39,39,39)',(#19985));
#19980=FILL_AREA_STYLE_COLOUR('Steel - Satin',#19986);
#19981=FILL_AREA_STYLE_COLOUR('Opaque(203,203,203)',#19987);
#19982=FILL_AREA_STYLE_COLOUR('Opaque(160,160,160)',#19988);
#19983=FILL_AREA_STYLE_COLOUR('Opaque(255,85,127)',#19989);
#19984=FILL_AREA_STYLE_COLOUR('Opaque(170,0,255)',#19990);
#19985=FILL_AREA_STYLE_COLOUR('Opaque(39,39,39)',#19991);
#19986=COLOUR_RGB('Steel - Satin', 0.09019608, 0.27058824, 0.51372549);
#19987=COLOUR_RGB('Opaque(203,203,203)', 0.09019608, 0.27058824, 0.51372549);
#19988=COLOUR_RGB('Opaque(160,160,160)', 0.66274510, 0.83137255, 0.94901961);
#19989=COLOUR_RGB('Opaque(255,85,127)', 0.40784314, 0.44705882, 0.49803922);
#19990=COLOUR_RGB('Opaque(170,0,255)', 0.72549020, 0.75294118, 0.79215686);
#19991=COLOUR_RGB('Opaque(39,39,39)', 0.09019608, 0.27058824, 0.51372549);
ENDSEC;
END-ISO-10303-21;
